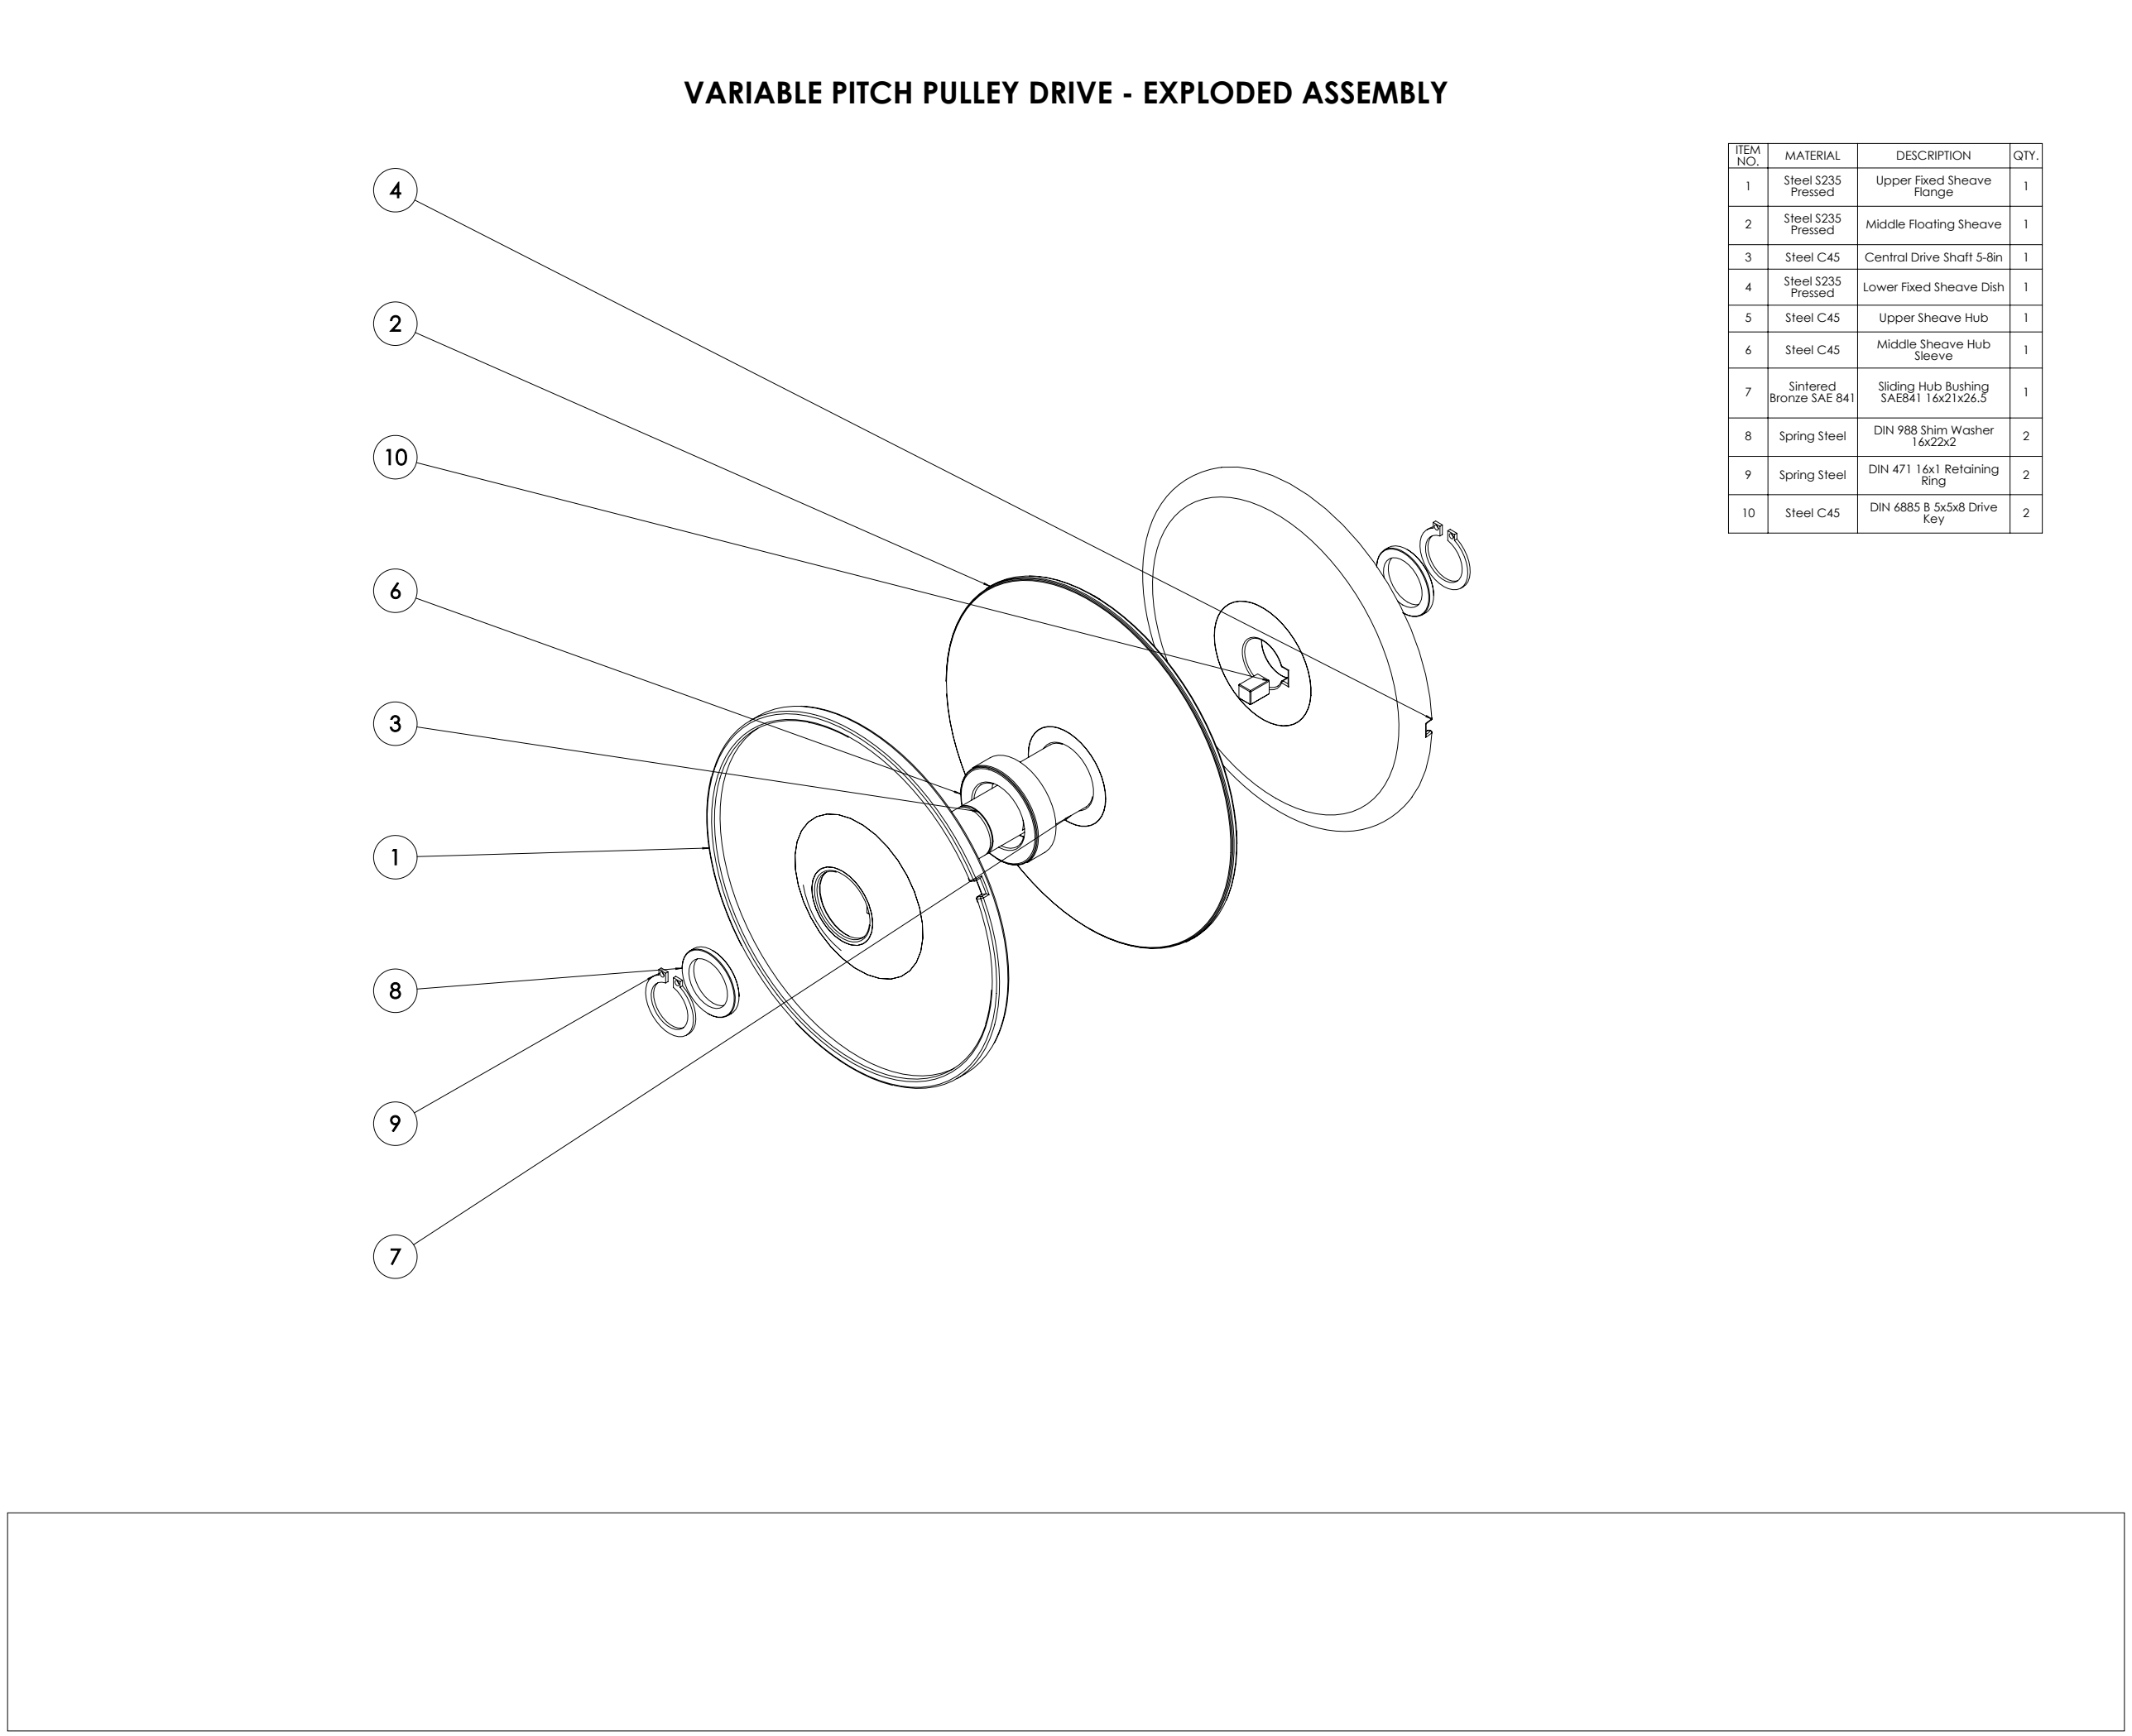
ISO-10303-21;
HEADER;
/* Generated by software containing ST-Developer
 * from STEP Tools, Inc. (www.steptools.com) 
 */

FILE_DESCRIPTION(
/* description */ (''),
/* implementation_level */ '2;1');

FILE_NAME(
/* name */ 'MAS-362',
/* time_stamp */ '2026-10-24T13:41:11-07:00',
/* author */ (''),
/* organization */ (''),
/* preprocessor_version */ 'ST-DEVELOPER v20.2',
/* originating_system */ 'Autodesk Translation Framework v15.15.0.0',
/* authorisation */ '');

FILE_SCHEMA (('AUTOMOTIVE_DESIGN { 1 0 10303 214 3 1 1 }'));
ENDSEC;

DATA;
#10=MECHANICAL_DESIGN_GEOMETRIC_PRESENTATION_REPRESENTATION('',(#121,#122,
#123,#124,#125,#126,#127,#128,#129,#130),#12813);
#11=ITEM_DEFINED_TRANSFORMATION($,$,#4506,#4991);
#12=ITEM_DEFINED_TRANSFORMATION($,$,#4561,#4992);
#13=ITEM_DEFINED_TRANSFORMATION($,$,#4614,#4993);
#14=ITEM_DEFINED_TRANSFORMATION($,$,#4704,#4994);
#15=ITEM_DEFINED_TRANSFORMATION($,$,#4796,#4995);
#16=ITEM_DEFINED_TRANSFORMATION($,$,#4885,#4996);
#17=ITEM_DEFINED_TRANSFORMATION($,$,#4917,#4997);
#18=ITEM_DEFINED_TRANSFORMATION($,$,#4930,#4998);
#19=ITEM_DEFINED_TRANSFORMATION($,$,#4930,#4999);
#20=ITEM_DEFINED_TRANSFORMATION($,$,#4943,#5000);
#21=ITEM_DEFINED_TRANSFORMATION($,$,#4943,#5001);
#22=ITEM_DEFINED_TRANSFORMATION($,$,#4964,#5002);
#23=ITEM_DEFINED_TRANSFORMATION($,$,#4964,#5003);
#24=(
REPRESENTATION_RELATIONSHIP($,$,#12854,#12853)
REPRESENTATION_RELATIONSHIP_WITH_TRANSFORMATION(#11)
SHAPE_REPRESENTATION_RELATIONSHIP()
);
#25=(
REPRESENTATION_RELATIONSHIP($,$,#12855,#12853)
REPRESENTATION_RELATIONSHIP_WITH_TRANSFORMATION(#12)
SHAPE_REPRESENTATION_RELATIONSHIP()
);
#26=(
REPRESENTATION_RELATIONSHIP($,$,#12856,#12853)
REPRESENTATION_RELATIONSHIP_WITH_TRANSFORMATION(#13)
SHAPE_REPRESENTATION_RELATIONSHIP()
);
#27=(
REPRESENTATION_RELATIONSHIP($,$,#12857,#12853)
REPRESENTATION_RELATIONSHIP_WITH_TRANSFORMATION(#14)
SHAPE_REPRESENTATION_RELATIONSHIP()
);
#28=(
REPRESENTATION_RELATIONSHIP($,$,#12858,#12853)
REPRESENTATION_RELATIONSHIP_WITH_TRANSFORMATION(#15)
SHAPE_REPRESENTATION_RELATIONSHIP()
);
#29=(
REPRESENTATION_RELATIONSHIP($,$,#12859,#12853)
REPRESENTATION_RELATIONSHIP_WITH_TRANSFORMATION(#16)
SHAPE_REPRESENTATION_RELATIONSHIP()
);
#30=(
REPRESENTATION_RELATIONSHIP($,$,#12860,#12853)
REPRESENTATION_RELATIONSHIP_WITH_TRANSFORMATION(#17)
SHAPE_REPRESENTATION_RELATIONSHIP()
);
#31=(
REPRESENTATION_RELATIONSHIP($,$,#12861,#12853)
REPRESENTATION_RELATIONSHIP_WITH_TRANSFORMATION(#18)
SHAPE_REPRESENTATION_RELATIONSHIP()
);
#32=(
REPRESENTATION_RELATIONSHIP($,$,#12861,#12853)
REPRESENTATION_RELATIONSHIP_WITH_TRANSFORMATION(#19)
SHAPE_REPRESENTATION_RELATIONSHIP()
);
#33=(
REPRESENTATION_RELATIONSHIP($,$,#12862,#12853)
REPRESENTATION_RELATIONSHIP_WITH_TRANSFORMATION(#20)
SHAPE_REPRESENTATION_RELATIONSHIP()
);
#34=(
REPRESENTATION_RELATIONSHIP($,$,#12862,#12853)
REPRESENTATION_RELATIONSHIP_WITH_TRANSFORMATION(#21)
SHAPE_REPRESENTATION_RELATIONSHIP()
);
#35=(
REPRESENTATION_RELATIONSHIP($,$,#12863,#12853)
REPRESENTATION_RELATIONSHIP_WITH_TRANSFORMATION(#22)
SHAPE_REPRESENTATION_RELATIONSHIP()
);
#36=(
REPRESENTATION_RELATIONSHIP($,$,#12863,#12853)
REPRESENTATION_RELATIONSHIP_WITH_TRANSFORMATION(#23)
SHAPE_REPRESENTATION_RELATIONSHIP()
);
#37=CONTEXT_DEPENDENT_SHAPE_REPRESENTATION(#24,#12840);
#38=CONTEXT_DEPENDENT_SHAPE_REPRESENTATION(#25,#12841);
#39=CONTEXT_DEPENDENT_SHAPE_REPRESENTATION(#26,#12842);
#40=CONTEXT_DEPENDENT_SHAPE_REPRESENTATION(#27,#12843);
#41=CONTEXT_DEPENDENT_SHAPE_REPRESENTATION(#28,#12844);
#42=CONTEXT_DEPENDENT_SHAPE_REPRESENTATION(#29,#12845);
#43=CONTEXT_DEPENDENT_SHAPE_REPRESENTATION(#30,#12846);
#44=CONTEXT_DEPENDENT_SHAPE_REPRESENTATION(#31,#12847);
#45=CONTEXT_DEPENDENT_SHAPE_REPRESENTATION(#32,#12848);
#46=CONTEXT_DEPENDENT_SHAPE_REPRESENTATION(#33,#12849);
#47=CONTEXT_DEPENDENT_SHAPE_REPRESENTATION(#34,#12850);
#48=CONTEXT_DEPENDENT_SHAPE_REPRESENTATION(#35,#12851);
#49=CONTEXT_DEPENDENT_SHAPE_REPRESENTATION(#36,#12852);
#50=NEXT_ASSEMBLY_USAGE_OCCURRENCE('01_Upper_Fixed_Sheave_Flange:2',
'01_Upper_Fixed_Sheave_Flange:2','01_Upper_Fixed_Sheave_Flange:2',#12865,
#12866,'01_Upper_Fixed_Sheave_Flange:2');
#51=NEXT_ASSEMBLY_USAGE_OCCURRENCE('02_Middle_Floating_Sheave:2',
'02_Middle_Floating_Sheave:2','02_Middle_Floating_Sheave:2',#12865,#12867,
'02_Middle_Floating_Sheave:2');
#52=NEXT_ASSEMBLY_USAGE_OCCURRENCE('03_Central_Drive_Shaft_5-8in:2',
'03_Central_Drive_Shaft_5-8in:2','03_Central_Drive_Shaft_5-8in:2',#12865,
#12868,'03_Central_Drive_Shaft_5-8in:2');
#53=NEXT_ASSEMBLY_USAGE_OCCURRENCE('04_Lower_Fixed_Sheave_Dish:2',
'04_Lower_Fixed_Sheave_Dish:2','04_Lower_Fixed_Sheave_Dish:2',#12865,#12869,
'04_Lower_Fixed_Sheave_Dish:2');
#54=NEXT_ASSEMBLY_USAGE_OCCURRENCE('05_Upper_Sheave_Hub:2',
'05_Upper_Sheave_Hub:2','05_Upper_Sheave_Hub:2',#12865,#12870,
'05_Upper_Sheave_Hub:2');
#55=NEXT_ASSEMBLY_USAGE_OCCURRENCE('06_Middle_Sheave_Hub_Sleeve:2',
'06_Middle_Sheave_Hub_Sleeve:2','06_Middle_Sheave_Hub_Sleeve:2',#12865,
#12871,'06_Middle_Sheave_Hub_Sleeve:2');
#56=NEXT_ASSEMBLY_USAGE_OCCURRENCE(
'07_Sliding_Hub_Bushing_SAE841_16x21x26.5:2',
'07_Sliding_Hub_Bushing_SAE841_16x21x26.5:2',
'07_Sliding_Hub_Bushing_SAE841_16x21x26.5:2',#12865,#12872,
'07_Sliding_Hub_Bushing_SAE841_16x21x26.5:2');
#57=NEXT_ASSEMBLY_USAGE_OCCURRENCE('08_DIN_988_Shim_Washer_16x22x2:2',
'08_DIN_988_Shim_Washer_16x22x2:2','08_DIN_988_Shim_Washer_16x22x2:2',#12865,
#12873,'08_DIN_988_Shim_Washer_16x22x2:2');
#58=NEXT_ASSEMBLY_USAGE_OCCURRENCE('08_DIN_988_Shim_Washer_16x22x2:3',
'08_DIN_988_Shim_Washer_16x22x2:3','08_DIN_988_Shim_Washer_16x22x2:3',#12865,
#12873,'08_DIN_988_Shim_Washer_16x22x2:3');
#59=NEXT_ASSEMBLY_USAGE_OCCURRENCE('09_DIN_471_16x1_Retaining_Ring:2',
'09_DIN_471_16x1_Retaining_Ring:2','09_DIN_471_16x1_Retaining_Ring:2',#12865,
#12874,'09_DIN_471_16x1_Retaining_Ring:2');
#60=NEXT_ASSEMBLY_USAGE_OCCURRENCE('09_DIN_471_16x1_Retaining_Ring:3',
'09_DIN_471_16x1_Retaining_Ring:3','09_DIN_471_16x1_Retaining_Ring:3',#12865,
#12874,'09_DIN_471_16x1_Retaining_Ring:3');
#61=NEXT_ASSEMBLY_USAGE_OCCURRENCE('10_DIN_6885_B_5x5x8_Drive_Key:2',
'10_DIN_6885_B_5x5x8_Drive_Key:2','10_DIN_6885_B_5x5x8_Drive_Key:2',#12865,
#12875,'10_DIN_6885_B_5x5x8_Drive_Key:2');
#62=NEXT_ASSEMBLY_USAGE_OCCURRENCE('10_DIN_6885_B_5x5x8_Drive_Key:3',
'10_DIN_6885_B_5x5x8_Drive_Key:3','10_DIN_6885_B_5x5x8_Drive_Key:3',#12865,
#12875,'10_DIN_6885_B_5x5x8_Drive_Key:3');
#63=ELLIPSE('',#4739,0.707106781186547,0.5);
#64=ELLIPSE('',#4740,0.707106781186547,0.5);
#65=ELLIPSE('',#4754,0.707106781186549,0.5);
#66=ELLIPSE('',#4755,0.707106781186547,0.5);
#67=SPHERICAL_SURFACE('',#4710,0.5);
#68=SPHERICAL_SURFACE('',#4712,0.5);
#69=SPHERICAL_SURFACE('',#4720,0.5);
#70=SPHERICAL_SURFACE('',#4723,0.5);
#71=SPHERICAL_SURFACE('',#4743,0.5);
#72=SPHERICAL_SURFACE('',#4756,0.5);
#73=SPHERICAL_SURFACE('',#4773,0.5);
#74=SPHERICAL_SURFACE('',#4779,0.5);
#75=SPHERICAL_SURFACE('',#4788,0.5);
#76=SPHERICAL_SURFACE('',#4790,0.5);
#77=SPHERICAL_SURFACE('',#4848,0.4);
#78=SPHERICAL_SURFACE('',#4850,0.4);
#79=SPHERICAL_SURFACE('',#4873,0.4);
#80=SPHERICAL_SURFACE('',#4876,0.4);
#81=CONICAL_SURFACE('',#4567,37.5,1.36447243276518);
#82=CONICAL_SURFACE('',#4576,59.25,0.785398163397448);
#83=CONICAL_SURFACE('',#4590,59.25,0.785398163397448);
#84=CONICAL_SURFACE('',#4597,37.5,1.39585880542621);
#85=CONICAL_SURFACE('',#4661,1.775,1.02974425867666);
#86=CONICAL_SURFACE('',#4663,3.85,0.785398163397459);
#87=CONICAL_SURFACE('',#4698,7.69,0.785398163397449);
#88=CONICAL_SURFACE('',#4701,7.54,0.785398163397436);
#89=CONICAL_SURFACE('',#4727,35.,1.37340076694502);
#90=CONICAL_SURFACE('',#4770,35.5,1.39833325526807);
#91=CONICAL_SURFACE('',#4795,56.05,0.694738276196701);
#92=CONICAL_SURFACE('',#4797,12.45,0.785398163397445);
#93=CONICAL_SURFACE('',#4806,12.45,0.785398163397445);
#94=CONICAL_SURFACE('',#4828,10.75,0.785398163397451);
#95=CONICAL_SURFACE('',#4840,10.75,0.785398163397451);
#96=CONICAL_SURFACE('',#4891,15.75,0.785398163397451);
#97=CONICAL_SURFACE('',#4923,8.115,0.785398163397445);
#98=CONICAL_SURFACE('',#4927,8.115,0.785398163397448);
#99=CONICAL_SURFACE('',#4931,10.9,0.785398163397449);
#100=CONICAL_SURFACE('',#4936,10.9,0.785398163397448);
#101=SHAPE_REPRESENTATION_RELATIONSHIP('SRR','None',#12854,#111);
#102=SHAPE_REPRESENTATION_RELATIONSHIP('SRR','None',#12855,#112);
#103=SHAPE_REPRESENTATION_RELATIONSHIP('SRR','None',#12856,#113);
#104=SHAPE_REPRESENTATION_RELATIONSHIP('SRR','None',#12857,#114);
#105=SHAPE_REPRESENTATION_RELATIONSHIP('SRR','None',#12858,#115);
#106=SHAPE_REPRESENTATION_RELATIONSHIP('SRR','None',#12859,#116);
#107=SHAPE_REPRESENTATION_RELATIONSHIP('SRR','None',#12860,#117);
#108=SHAPE_REPRESENTATION_RELATIONSHIP('SRR','None',#12861,#118);
#109=SHAPE_REPRESENTATION_RELATIONSHIP('SRR','None',#12862,#119);
#110=SHAPE_REPRESENTATION_RELATIONSHIP('SRR','None',#12863,#120);
#111=ADVANCED_BREP_SHAPE_REPRESENTATION('',(#131),#12803);
#112=ADVANCED_BREP_SHAPE_REPRESENTATION('',(#132),#12804);
#113=ADVANCED_BREP_SHAPE_REPRESENTATION('',(#133),#12805);
#114=ADVANCED_BREP_SHAPE_REPRESENTATION('',(#134),#12806);
#115=ADVANCED_BREP_SHAPE_REPRESENTATION('',(#135),#12807);
#116=ADVANCED_BREP_SHAPE_REPRESENTATION('',(#136),#12808);
#117=ADVANCED_BREP_SHAPE_REPRESENTATION('',(#137),#12809);
#118=ADVANCED_BREP_SHAPE_REPRESENTATION('',(#138),#12810);
#119=ADVANCED_BREP_SHAPE_REPRESENTATION('',(#139),#12811);
#120=ADVANCED_BREP_SHAPE_REPRESENTATION('',(#140),#12812);
#121=STYLED_ITEM('',(#12960),#131);
#122=STYLED_ITEM('',(#12988),#132);
#123=STYLED_ITEM('',(#12974),#133);
#124=STYLED_ITEM('',(#12967),#134);
#125=STYLED_ITEM('',(#12960),#135);
#126=STYLED_ITEM('',(#12960),#136);
#127=STYLED_ITEM('',(#12967),#137);
#128=STYLED_ITEM('',(#12981),#138);
#129=STYLED_ITEM('',(#12988),#139);
#130=STYLED_ITEM('',(#12974),#140);
#131=MANIFOLD_SOLID_BREP('Body1',#4384);
#132=MANIFOLD_SOLID_BREP('Body1',#4385);
#133=MANIFOLD_SOLID_BREP('Body1',#4386);
#134=MANIFOLD_SOLID_BREP('Body1',#4387);
#135=MANIFOLD_SOLID_BREP('Body1',#4388);
#136=MANIFOLD_SOLID_BREP('Body1',#4389);
#137=MANIFOLD_SOLID_BREP('Body1',#4390);
#138=MANIFOLD_SOLID_BREP('Body1',#4391);
#139=MANIFOLD_SOLID_BREP('Body1',#4392);
#140=MANIFOLD_SOLID_BREP('Body1',#4393);
#141=FACE_BOUND('',#599,.T.);
#142=FACE_BOUND('',#604,.T.);
#143=FACE_BOUND('',#607,.T.);
#144=FACE_BOUND('',#632,.T.);
#145=FACE_BOUND('',#643,.T.);
#146=FACE_BOUND('',#701,.T.);
#147=FACE_BOUND('',#704,.T.);
#148=FACE_BOUND('',#706,.T.);
#149=FACE_BOUND('',#707,.T.);
#150=FACE_BOUND('',#709,.T.);
#151=FACE_BOUND('',#712,.T.);
#152=FACE_BOUND('',#719,.T.);
#153=FACE_BOUND('',#738,.T.);
#154=FACE_BOUND('',#753,.T.);
#155=FACE_BOUND('',#774,.T.);
#156=FACE_BOUND('',#779,.T.);
#157=FACE_BOUND('',#782,.T.);
#158=FACE_BOUND('',#811,.T.);
#159=FACE_BOUND('',#825,.T.);
#160=FACE_BOUND('',#830,.T.);
#161=FACE_BOUND('',#836,.T.);
#162=FACE_BOUND('',#841,.T.);
#163=FACE_BOUND('',#846,.T.);
#164=FACE_BOUND('',#849,.T.);
#165=FACE_BOUND('',#853,.T.);
#166=FACE_BOUND('',#854,.T.);
#167=FACE_BOUND('',#859,.T.);
#168=FACE_BOUND('',#860,.T.);
#169=PLANE('',#4514);
#170=PLANE('',#4517);
#171=PLANE('',#4521);
#172=PLANE('',#4531);
#173=PLANE('',#4540);
#174=PLANE('',#4544);
#175=PLANE('',#4551);
#176=PLANE('',#4570);
#177=PLANE('',#4603);
#178=PLANE('',#4654);
#179=PLANE('',#4658);
#180=PLANE('',#4665);
#181=PLANE('',#4666);
#182=PLANE('',#4668);
#183=PLANE('',#4669);
#184=PLANE('',#4671);
#185=PLANE('',#4672);
#186=PLANE('',#4673);
#187=PLANE('',#4675);
#188=PLANE('',#4676);
#189=PLANE('',#4678);
#190=PLANE('',#4679);
#191=PLANE('',#4684);
#192=PLANE('',#4688);
#193=PLANE('',#4692);
#194=PLANE('',#4696);
#195=PLANE('',#4703);
#196=PLANE('',#4717);
#197=PLANE('',#4725);
#198=PLANE('',#4734);
#199=PLANE('',#4751);
#200=PLANE('',#4752);
#201=PLANE('',#4769);
#202=PLANE('',#4781);
#203=PLANE('',#4792);
#204=PLANE('',#4793);
#205=PLANE('',#4794);
#206=PLANE('',#4804);
#207=PLANE('',#4808);
#208=PLANE('',#4816);
#209=PLANE('',#4817);
#210=PLANE('',#4818);
#211=PLANE('',#4819);
#212=PLANE('',#4820);
#213=PLANE('',#4852);
#214=PLANE('',#4855);
#215=PLANE('',#4862);
#216=PLANE('',#4872);
#217=PLANE('',#4884);
#218=PLANE('',#4894);
#219=PLANE('',#4906);
#220=PLANE('',#4921);
#221=PLANE('',#4929);
#222=PLANE('',#4938);
#223=PLANE('',#4942);
#224=PLANE('',#4950);
#225=PLANE('',#4953);
#226=PLANE('',#4954);
#227=PLANE('',#4955);
#228=PLANE('',#4956);
#229=PLANE('',#4960);
#230=PLANE('',#4961);
#231=PLANE('',#4962);
#232=PLANE('',#4965);
#233=PLANE('',#4966);
#234=PLANE('',#4967);
#235=PLANE('',#4968);
#236=PLANE('',#4969);
#237=PLANE('',#4970);
#238=PLANE('',#4971);
#239=PLANE('',#4972);
#240=PLANE('',#4973);
#241=PLANE('',#4974);
#242=PLANE('',#4975);
#243=PLANE('',#4976);
#244=PLANE('',#4977);
#245=PLANE('',#4978);
#246=PLANE('',#4979);
#247=PLANE('',#4980);
#248=PLANE('',#4981);
#249=PLANE('',#4982);
#250=PLANE('',#4983);
#251=PLANE('',#4984);
#252=PLANE('',#4985);
#253=PLANE('',#4986);
#254=PLANE('',#4987);
#255=PLANE('',#4988);
#256=PLANE('',#4989);
#257=PLANE('',#4990);
#258=TOROIDAL_SURFACE('',#4511,11.5,0.5);
#259=TOROIDAL_SURFACE('',#4541,60.,0.5);
#260=TOROIDAL_SURFACE('',#4546,58.,0.5);
#261=TOROIDAL_SURFACE('',#4549,58.1,0.6);
#262=TOROIDAL_SURFACE('',#4558,59.9,0.6);
#263=TOROIDAL_SURFACE('',#4559,59.7,0.8);
#264=TOROIDAL_SURFACE('',#4562,15.9482352626124,0.5);
#265=TOROIDAL_SURFACE('',#4572,58.7517732660432,0.5);
#266=TOROIDAL_SURFACE('',#4579,59.,0.5);
#267=TOROIDAL_SURFACE('',#4586,59.,0.5);
#268=TOROIDAL_SURFACE('',#4593,58.7578429367487,0.5);
#269=TOROIDAL_SURFACE('',#4600,15.9561537431677,0.5);
#270=TOROIDAL_SURFACE('',#4605,11.,0.5);
#271=TOROIDAL_SURFACE('',#4612,11.,0.5);
#272=TOROIDAL_SURFACE('',#4705,56.5341874729922,0.5);
#273=TOROIDAL_SURFACE('',#4729,11.5,0.5);
#274=TOROIDAL_SURFACE('',#4746,8.45,0.5);
#275=TOROIDAL_SURFACE('',#4760,8.45,0.5);
#276=TOROIDAL_SURFACE('',#4764,19.9567770454363,0.5);
#277=TOROIDAL_SURFACE('',#4821,10.6,0.4);
#278=TOROIDAL_SURFACE('',#4831,10.6,0.4);
#279=TOROIDAL_SURFACE('',#4838,10.6,0.4);
#280=TOROIDAL_SURFACE('',#4844,10.3343145750508,0.4);
#281=TOROIDAL_SURFACE('',#4859,10.3343145750508,0.4);
#282=TOROIDAL_SURFACE('',#4864,8.35,0.4);
#283=TOROIDAL_SURFACE('',#4879,8.35,0.4);
#284=TOROIDAL_SURFACE('',#4881,8.35,0.4);
#285=TOROIDAL_SURFACE('',#4886,15.2928932188134,0.5);
#286=TOROIDAL_SURFACE('',#4896,15.5,0.5);
#287=TOROIDAL_SURFACE('',#4903,15.5,0.5);
#288=TOROIDAL_SURFACE('',#4908,11.,0.5);
#289=TOROIDAL_SURFACE('',#4915,11.,0.5);
#290=(
BOUNDED_CURVE()
B_SPLINE_CURVE(5,(#6647,#6648,#6649,#6650,#6651,#6652,#6653,#6654,#6655,
#6656,#6657,#6658,#6659,#6660,#6661,#6662,#6663,#6664,#6665,#6666,#6667,
#6668,#6669,#6670,#6671,#6672,#6673,#6674,#6675,#6676),.UNSPECIFIED.,.F.,
 .F.)
B_SPLINE_CURVE_WITH_KNOTS((6,1,1,1,1,1,1,1,1,1,1,1,1,1,1,1,1,1,1,1,1,1,
1,1,1,6),(8.37815962158244E-5,0.04,0.08,0.12,0.16,0.2,0.24,0.28,0.32,0.36,
0.4,0.44,0.48,0.52,0.56,0.6,0.64,0.68,0.72,0.76,0.8,0.84,0.88,0.92,0.96,
0.969915757295795),.UNSPECIFIED.)
CURVE()
GEOMETRIC_REPRESENTATION_ITEM()
RATIONAL_B_SPLINE_CURVE((1.,1.,1.,1.,1.,1.,1.,1.,1.,1.,1.,1.,1.,1.,1.,1.,
1.,1.,1.,1.,1.,1.,1.,1.,1.,1.,1.,1.,1.,1.))
REPRESENTATION_ITEM('')
);
#291=(
BOUNDED_CURVE()
B_SPLINE_CURVE(5,(#7077,#7078,#7079,#7080,#7081,#7082,#7083,#7084,#7085,
#7086,#7087,#7088,#7089,#7090,#7091,#7092,#7093,#7094,#7095,#7096,#7097,
#7098,#7099,#7100,#7101,#7102,#7103,#7104,#7105,#7106),.UNSPECIFIED.,.F.,
 .F.)
B_SPLINE_CURVE_WITH_KNOTS((6,1,1,1,1,1,1,1,1,1,1,1,1,1,1,1,1,1,1,1,1,1,
1,1,1,6),(0.00142562377953934,0.04,0.08,0.12,0.16,0.2,0.24,0.28,0.32,0.36,
0.4,0.44,0.48,0.52,0.56,0.6,0.64,0.68,0.72,0.76,0.8,0.84,0.88,0.92,0.96,
0.999682925140619),.UNSPECIFIED.)
CURVE()
GEOMETRIC_REPRESENTATION_ITEM()
RATIONAL_B_SPLINE_CURVE((1.,1.,1.,1.,1.,1.,1.,1.,1.,1.,1.,1.,1.,1.,1.,1.,
1.,1.,1.,1.,1.,1.,1.,1.,1.,1.,1.,1.,1.,1.))
REPRESENTATION_ITEM('')
);
#292=(
BOUNDED_CURVE()
B_SPLINE_CURVE(5,(#10926,#10927,#10928,#10929,#10930,#10931,#10932,#10933,
#10934,#10935,#10936,#10937,#10938,#10939,#10940),.UNSPECIFIED.,.F.,.F.)
B_SPLINE_CURVE_WITH_KNOTS((6,1,1,1,1,1,1,1,1,1,6),(0.000900413620571326,
0.0666666666666667,0.133333333333333,0.2,0.266666666666667,0.333333333333333,
0.4,0.466666666666667,0.533333333333333,0.6,0.62572757688512),
 .UNSPECIFIED.)
CURVE()
GEOMETRIC_REPRESENTATION_ITEM()
RATIONAL_B_SPLINE_CURVE((1.,1.,1.,1.,1.,1.,1.,1.,1.,1.,1.,1.,1.,1.,1.))
REPRESENTATION_ITEM('')
);
#293=(
BOUNDED_CURVE()
B_SPLINE_CURVE(5,(#11656,#11657,#11658,#11659,#11660,#11661,#11662,#11663,
#11664,#11665,#11666,#11667,#11668,#11669,#11670,#11671,#11672,#11673,#11674),
 .UNSPECIFIED.,.F.,.F.)
B_SPLINE_CURVE_WITH_KNOTS((6,1,1,1,1,1,1,1,1,1,1,1,1,1,6),(0.323025444096601,
0.35,0.4,0.45,0.5,0.55,0.6,0.65,0.7,0.75,0.8,0.85,0.9,0.95,1.),
 .UNSPECIFIED.)
CURVE()
GEOMETRIC_REPRESENTATION_ITEM()
RATIONAL_B_SPLINE_CURVE((1.,1.,1.,1.,1.,1.,1.,1.,1.,1.,1.,1.,1.,1.,1.,1.,
1.,1.,1.))
REPRESENTATION_ITEM('')
);
#294=(
BOUNDED_SURFACE()
B_SPLINE_SURFACE(5,2,((#6376,#6377,#6378,#6379,#6380,#6381,#6382,#6383,
#6384),(#6385,#6386,#6387,#6388,#6389,#6390,#6391,#6392,#6393),(#6394,#6395,
#6396,#6397,#6398,#6399,#6400,#6401,#6402),(#6403,#6404,#6405,#6406,#6407,
#6408,#6409,#6410,#6411),(#6412,#6413,#6414,#6415,#6416,#6417,#6418,#6419,
#6420),(#6421,#6422,#6423,#6424,#6425,#6426,#6427,#6428,#6429),(#6430,#6431,
#6432,#6433,#6434,#6435,#6436,#6437,#6438),(#6439,#6440,#6441,#6442,#6443,
#6444,#6445,#6446,#6447),(#6448,#6449,#6450,#6451,#6452,#6453,#6454,#6455,
#6456),(#6457,#6458,#6459,#6460,#6461,#6462,#6463,#6464,#6465),(#6466,#6467,
#6468,#6469,#6470,#6471,#6472,#6473,#6474),(#6475,#6476,#6477,#6478,#6479,
#6480,#6481,#6482,#6483),(#6484,#6485,#6486,#6487,#6488,#6489,#6490,#6491,
#6492),(#6493,#6494,#6495,#6496,#6497,#6498,#6499,#6500,#6501),(#6502,#6503,
#6504,#6505,#6506,#6507,#6508,#6509,#6510),(#6511,#6512,#6513,#6514,#6515,
#6516,#6517,#6518,#6519),(#6520,#6521,#6522,#6523,#6524,#6525,#6526,#6527,
#6528),(#6529,#6530,#6531,#6532,#6533,#6534,#6535,#6536,#6537),(#6538,#6539,
#6540,#6541,#6542,#6543,#6544,#6545,#6546),(#6547,#6548,#6549,#6550,#6551,
#6552,#6553,#6554,#6555),(#6556,#6557,#6558,#6559,#6560,#6561,#6562,#6563,
#6564),(#6565,#6566,#6567,#6568,#6569,#6570,#6571,#6572,#6573),(#6574,#6575,
#6576,#6577,#6578,#6579,#6580,#6581,#6582),(#6583,#6584,#6585,#6586,#6587,
#6588,#6589,#6590,#6591),(#6592,#6593,#6594,#6595,#6596,#6597,#6598,#6599,
#6600),(#6601,#6602,#6603,#6604,#6605,#6606,#6607,#6608,#6609),(#6610,#6611,
#6612,#6613,#6614,#6615,#6616,#6617,#6618),(#6619,#6620,#6621,#6622,#6623,
#6624,#6625,#6626,#6627),(#6628,#6629,#6630,#6631,#6632,#6633,#6634,#6635,
#6636),(#6637,#6638,#6639,#6640,#6641,#6642,#6643,#6644,#6645)),
 .UNSPECIFIED.,.F.,.T.,.F.)
B_SPLINE_SURFACE_WITH_KNOTS((6,1,1,1,1,1,1,1,1,1,1,1,1,1,1,1,1,1,1,1,1,
1,1,1,1,6),(3,2,2,2,3),(0.,0.04,0.08,0.12,0.16,0.2,0.24,0.28,0.32,0.36,
0.4,0.44,0.48,0.52,0.56,0.6,0.64,0.68,0.72,0.76,0.8,0.84,0.88,0.92,0.96,
1.),(0.,1.5707963267949,3.14159265358979,4.71238898038469,6.28318530717959),
 .UNSPECIFIED.)
GEOMETRIC_REPRESENTATION_ITEM()
RATIONAL_B_SPLINE_SURFACE(((1.,0.707106781186548,1.,0.707106781186548,1.,
0.707106781186548,1.,0.707106781186548,1.),(1.,0.707106781186548,1.,0.707106781186548,
1.,0.707106781186548,1.,0.707106781186548,1.),(1.,0.707106781186548,1.,
0.707106781186548,1.,0.707106781186548,1.,0.707106781186548,1.),(1.,0.707106781186548,
1.,0.707106781186548,1.,0.707106781186548,1.,0.707106781186548,1.),(1.,
0.707106781186548,1.,0.707106781186548,1.,0.707106781186548,1.,0.707106781186548,
1.),(1.,0.707106781186548,1.,0.707106781186548,1.,0.707106781186548,1.,
0.707106781186548,1.),(1.,0.707106781186548,1.,0.707106781186548,1.,0.707106781186548,
1.,0.707106781186548,1.),(1.,0.707106781186548,1.,0.707106781186548,1.,
0.707106781186548,1.,0.707106781186548,1.),(1.,0.707106781186548,1.,0.707106781186548,
1.,0.707106781186548,1.,0.707106781186548,1.),(1.,0.707106781186548,1.,
0.707106781186548,1.,0.707106781186548,1.,0.707106781186548,1.),(1.,0.707106781186548,
1.,0.707106781186548,1.,0.707106781186548,1.,0.707106781186548,1.),(1.,
0.707106781186548,1.,0.707106781186548,1.,0.707106781186548,1.,0.707106781186548,
1.),(1.,0.707106781186548,1.,0.707106781186548,1.,0.707106781186548,1.,
0.707106781186548,1.),(1.,0.707106781186548,1.,0.707106781186548,1.,0.707106781186548,
1.,0.707106781186548,1.),(1.,0.707106781186548,1.,0.707106781186548,1.,
0.707106781186548,1.,0.707106781186548,1.),(1.,0.707106781186548,1.,0.707106781186548,
1.,0.707106781186548,1.,0.707106781186548,1.),(1.,0.707106781186548,1.,
0.707106781186548,1.,0.707106781186548,1.,0.707106781186548,1.),(1.,0.707106781186548,
1.,0.707106781186548,1.,0.707106781186548,1.,0.707106781186548,1.),(1.,
0.707106781186548,1.,0.707106781186548,1.,0.707106781186548,1.,0.707106781186548,
1.),(1.,0.707106781186548,1.,0.707106781186548,1.,0.707106781186548,1.,
0.707106781186548,1.),(1.,0.707106781186548,1.,0.707106781186548,1.,0.707106781186548,
1.,0.707106781186548,1.),(1.,0.707106781186548,1.,0.707106781186548,1.,
0.707106781186548,1.,0.707106781186548,1.),(1.,0.707106781186548,1.,0.707106781186548,
1.,0.707106781186548,1.,0.707106781186548,1.),(1.,0.707106781186548,1.,
0.707106781186548,1.,0.707106781186548,1.,0.707106781186548,1.),(1.,0.707106781186548,
1.,0.707106781186548,1.,0.707106781186548,1.,0.707106781186548,1.),(1.,
0.707106781186548,1.,0.707106781186548,1.,0.707106781186548,1.,0.707106781186548,
1.),(1.,0.707106781186548,1.,0.707106781186548,1.,0.707106781186548,1.,
0.707106781186548,1.),(1.,0.707106781186548,1.,0.707106781186548,1.,0.707106781186548,
1.,0.707106781186548,1.),(1.,0.707106781186548,1.,0.707106781186548,1.,
0.707106781186548,1.,0.707106781186548,1.),(1.,0.707106781186548,1.,0.707106781186548,
1.,0.707106781186548,1.,0.707106781186548,1.)))
REPRESENTATION_ITEM('')
SURFACE()
);
#295=(
BOUNDED_SURFACE()
B_SPLINE_SURFACE(5,2,((#6806,#6807,#6808,#6809,#6810,#6811,#6812,#6813,
#6814),(#6815,#6816,#6817,#6818,#6819,#6820,#6821,#6822,#6823),(#6824,#6825,
#6826,#6827,#6828,#6829,#6830,#6831,#6832),(#6833,#6834,#6835,#6836,#6837,
#6838,#6839,#6840,#6841),(#6842,#6843,#6844,#6845,#6846,#6847,#6848,#6849,
#6850),(#6851,#6852,#6853,#6854,#6855,#6856,#6857,#6858,#6859),(#6860,#6861,
#6862,#6863,#6864,#6865,#6866,#6867,#6868),(#6869,#6870,#6871,#6872,#6873,
#6874,#6875,#6876,#6877),(#6878,#6879,#6880,#6881,#6882,#6883,#6884,#6885,
#6886),(#6887,#6888,#6889,#6890,#6891,#6892,#6893,#6894,#6895),(#6896,#6897,
#6898,#6899,#6900,#6901,#6902,#6903,#6904),(#6905,#6906,#6907,#6908,#6909,
#6910,#6911,#6912,#6913),(#6914,#6915,#6916,#6917,#6918,#6919,#6920,#6921,
#6922),(#6923,#6924,#6925,#6926,#6927,#6928,#6929,#6930,#6931),(#6932,#6933,
#6934,#6935,#6936,#6937,#6938,#6939,#6940),(#6941,#6942,#6943,#6944,#6945,
#6946,#6947,#6948,#6949),(#6950,#6951,#6952,#6953,#6954,#6955,#6956,#6957,
#6958),(#6959,#6960,#6961,#6962,#6963,#6964,#6965,#6966,#6967),(#6968,#6969,
#6970,#6971,#6972,#6973,#6974,#6975,#6976),(#6977,#6978,#6979,#6980,#6981,
#6982,#6983,#6984,#6985),(#6986,#6987,#6988,#6989,#6990,#6991,#6992,#6993,
#6994),(#6995,#6996,#6997,#6998,#6999,#7000,#7001,#7002,#7003),(#7004,#7005,
#7006,#7007,#7008,#7009,#7010,#7011,#7012),(#7013,#7014,#7015,#7016,#7017,
#7018,#7019,#7020,#7021),(#7022,#7023,#7024,#7025,#7026,#7027,#7028,#7029,
#7030),(#7031,#7032,#7033,#7034,#7035,#7036,#7037,#7038,#7039),(#7040,#7041,
#7042,#7043,#7044,#7045,#7046,#7047,#7048),(#7049,#7050,#7051,#7052,#7053,
#7054,#7055,#7056,#7057),(#7058,#7059,#7060,#7061,#7062,#7063,#7064,#7065,
#7066),(#7067,#7068,#7069,#7070,#7071,#7072,#7073,#7074,#7075)),
 .UNSPECIFIED.,.F.,.T.,.F.)
B_SPLINE_SURFACE_WITH_KNOTS((6,1,1,1,1,1,1,1,1,1,1,1,1,1,1,1,1,1,1,1,1,
1,1,1,1,6),(3,2,2,2,3),(0.,0.04,0.08,0.12,0.16,0.2,0.24,0.28,0.32,0.36,
0.4,0.44,0.48,0.52,0.56,0.6,0.64,0.68,0.72,0.76,0.8,0.84,0.88,0.92,0.96,
1.),(0.,1.5707963267949,3.14159265358979,4.71238898038469,6.28318530717959),
 .UNSPECIFIED.)
GEOMETRIC_REPRESENTATION_ITEM()
RATIONAL_B_SPLINE_SURFACE(((1.,0.707106781186548,1.,0.707106781186548,1.,
0.707106781186548,1.,0.707106781186548,1.),(1.,0.707106781186548,1.,0.707106781186548,
1.,0.707106781186548,1.,0.707106781186548,1.),(1.,0.707106781186548,1.,
0.707106781186548,1.,0.707106781186548,1.,0.707106781186548,1.),(1.,0.707106781186548,
1.,0.707106781186548,1.,0.707106781186548,1.,0.707106781186548,1.),(1.,
0.707106781186548,1.,0.707106781186548,1.,0.707106781186548,1.,0.707106781186548,
1.),(1.,0.707106781186548,1.,0.707106781186548,1.,0.707106781186548,1.,
0.707106781186548,1.),(1.,0.707106781186548,1.,0.707106781186548,1.,0.707106781186548,
1.,0.707106781186548,1.),(1.,0.707106781186548,1.,0.707106781186548,1.,
0.707106781186548,1.,0.707106781186548,1.),(1.,0.707106781186548,1.,0.707106781186548,
1.,0.707106781186548,1.,0.707106781186548,1.),(1.,0.707106781186548,1.,
0.707106781186548,1.,0.707106781186548,1.,0.707106781186548,1.),(1.,0.707106781186548,
1.,0.707106781186548,1.,0.707106781186548,1.,0.707106781186548,1.),(1.,
0.707106781186548,1.,0.707106781186548,1.,0.707106781186548,1.,0.707106781186548,
1.),(1.,0.707106781186548,1.,0.707106781186548,1.,0.707106781186548,1.,
0.707106781186548,1.),(1.,0.707106781186548,1.,0.707106781186548,1.,0.707106781186548,
1.,0.707106781186548,1.),(1.,0.707106781186548,1.,0.707106781186548,1.,
0.707106781186548,1.,0.707106781186548,1.),(1.,0.707106781186548,1.,0.707106781186548,
1.,0.707106781186548,1.,0.707106781186548,1.),(1.,0.707106781186548,1.,
0.707106781186548,1.,0.707106781186548,1.,0.707106781186548,1.),(1.,0.707106781186548,
1.,0.707106781186548,1.,0.707106781186548,1.,0.707106781186548,1.),(1.,
0.707106781186548,1.,0.707106781186548,1.,0.707106781186548,1.,0.707106781186548,
1.),(1.,0.707106781186548,1.,0.707106781186548,1.,0.707106781186548,1.,
0.707106781186548,1.),(1.,0.707106781186548,1.,0.707106781186548,1.,0.707106781186548,
1.,0.707106781186548,1.),(1.,0.707106781186548,1.,0.707106781186548,1.,
0.707106781186548,1.,0.707106781186548,1.),(1.,0.707106781186548,1.,0.707106781186548,
1.,0.707106781186548,1.,0.707106781186548,1.),(1.,0.707106781186548,1.,
0.707106781186548,1.,0.707106781186548,1.,0.707106781186548,1.),(1.,0.707106781186548,
1.,0.707106781186548,1.,0.707106781186548,1.,0.707106781186548,1.),(1.,
0.707106781186548,1.,0.707106781186548,1.,0.707106781186548,1.,0.707106781186548,
1.),(1.,0.707106781186548,1.,0.707106781186548,1.,0.707106781186548,1.,
0.707106781186548,1.),(1.,0.707106781186548,1.,0.707106781186548,1.,0.707106781186548,
1.,0.707106781186548,1.),(1.,0.707106781186548,1.,0.707106781186548,1.,
0.707106781186548,1.,0.707106781186548,1.),(1.,0.707106781186548,1.,0.707106781186548,
1.,0.707106781186548,1.,0.707106781186548,1.)))
REPRESENTATION_ITEM('')
SURFACE()
);
#296=(
BOUNDED_SURFACE()
B_SPLINE_SURFACE(5,2,((#10735,#10736,#10737,#10738,#10739,#10740,#10741,
#10742,#10743),(#10744,#10745,#10746,#10747,#10748,#10749,#10750,#10751,
#10752),(#10753,#10754,#10755,#10756,#10757,#10758,#10759,#10760,#10761),
(#10762,#10763,#10764,#10765,#10766,#10767,#10768,#10769,#10770),(#10771,
#10772,#10773,#10774,#10775,#10776,#10777,#10778,#10779),(#10780,#10781,
#10782,#10783,#10784,#10785,#10786,#10787,#10788),(#10789,#10790,#10791,
#10792,#10793,#10794,#10795,#10796,#10797),(#10798,#10799,#10800,#10801,
#10802,#10803,#10804,#10805,#10806),(#10807,#10808,#10809,#10810,#10811,
#10812,#10813,#10814,#10815),(#10816,#10817,#10818,#10819,#10820,#10821,
#10822,#10823,#10824),(#10825,#10826,#10827,#10828,#10829,#10830,#10831,
#10832,#10833),(#10834,#10835,#10836,#10837,#10838,#10839,#10840,#10841,
#10842),(#10843,#10844,#10845,#10846,#10847,#10848,#10849,#10850,#10851),
(#10852,#10853,#10854,#10855,#10856,#10857,#10858,#10859,#10860),(#10861,
#10862,#10863,#10864,#10865,#10866,#10867,#10868,#10869),(#10870,#10871,
#10872,#10873,#10874,#10875,#10876,#10877,#10878),(#10879,#10880,#10881,
#10882,#10883,#10884,#10885,#10886,#10887),(#10888,#10889,#10890,#10891,
#10892,#10893,#10894,#10895,#10896),(#10897,#10898,#10899,#10900,#10901,
#10902,#10903,#10904,#10905),(#10906,#10907,#10908,#10909,#10910,#10911,
#10912,#10913,#10914)),.UNSPECIFIED.,.F.,.T.,.F.)
B_SPLINE_SURFACE_WITH_KNOTS((6,1,1,1,1,1,1,1,1,1,1,1,1,1,1,6),(3,2,2,2,
3),(-1.,-0.933333333333333,-0.866666666666667,-0.8,-0.733333333333333,-0.666666666666667,
-0.6,-0.533333333333333,-0.466666666666667,-0.4,-0.333333333333333,-0.266666666666667,
-0.2,-0.133333333333333,-0.0666666666666667,0.),(0.,1.5707963267949,3.14159265358979,
4.71238898038469,6.28318530717959),.UNSPECIFIED.)
GEOMETRIC_REPRESENTATION_ITEM()
RATIONAL_B_SPLINE_SURFACE(((1.,0.707106781186548,1.,0.707106781186548,1.,
0.707106781186548,1.,0.707106781186548,1.),(1.,0.707106781186548,1.,0.707106781186548,
1.,0.707106781186548,1.,0.707106781186548,1.),(1.,0.707106781186548,1.,
0.707106781186548,1.,0.707106781186548,1.,0.707106781186548,1.),(1.,0.707106781186548,
1.,0.707106781186548,1.,0.707106781186548,1.,0.707106781186548,1.),(1.,
0.707106781186548,1.,0.707106781186548,1.,0.707106781186548,1.,0.707106781186548,
1.),(1.,0.707106781186548,1.,0.707106781186548,1.,0.707106781186548,1.,
0.707106781186548,1.),(1.,0.707106781186548,1.,0.707106781186548,1.,0.707106781186548,
1.,0.707106781186548,1.),(1.,0.707106781186548,1.,0.707106781186548,1.,
0.707106781186548,1.,0.707106781186548,1.),(1.,0.707106781186548,1.,0.707106781186548,
1.,0.707106781186548,1.,0.707106781186548,1.),(1.,0.707106781186548,1.,
0.707106781186548,1.,0.707106781186548,1.,0.707106781186548,1.),(1.,0.707106781186548,
1.,0.707106781186548,1.,0.707106781186548,1.,0.707106781186548,1.),(1.,
0.707106781186548,1.,0.707106781186548,1.,0.707106781186548,1.,0.707106781186548,
1.),(1.,0.707106781186548,1.,0.707106781186548,1.,0.707106781186548,1.,
0.707106781186548,1.),(1.,0.707106781186548,1.,0.707106781186548,1.,0.707106781186548,
1.,0.707106781186548,1.),(1.,0.707106781186548,1.,0.707106781186548,1.,
0.707106781186548,1.,0.707106781186548,1.),(1.,0.707106781186548,1.,0.707106781186548,
1.,0.707106781186548,1.,0.707106781186548,1.),(1.,0.707106781186548,1.,
0.707106781186548,1.,0.707106781186548,1.,0.707106781186548,1.),(1.,0.707106781186548,
1.,0.707106781186548,1.,0.707106781186548,1.,0.707106781186548,1.),(1.,
0.707106781186548,1.,0.707106781186548,1.,0.707106781186548,1.,0.707106781186548,
1.),(1.,0.707106781186548,1.,0.707106781186548,1.,0.707106781186548,1.,
0.707106781186548,1.)))
REPRESENTATION_ITEM('')
SURFACE()
);
#297=(
BOUNDED_SURFACE()
B_SPLINE_SURFACE(5,2,((#11421,#11422,#11423,#11424,#11425,#11426,#11427,
#11428,#11429),(#11430,#11431,#11432,#11433,#11434,#11435,#11436,#11437,
#11438),(#11439,#11440,#11441,#11442,#11443,#11444,#11445,#11446,#11447),
(#11448,#11449,#11450,#11451,#11452,#11453,#11454,#11455,#11456),(#11457,
#11458,#11459,#11460,#11461,#11462,#11463,#11464,#11465),(#11466,#11467,
#11468,#11469,#11470,#11471,#11472,#11473,#11474),(#11475,#11476,#11477,
#11478,#11479,#11480,#11481,#11482,#11483),(#11484,#11485,#11486,#11487,
#11488,#11489,#11490,#11491,#11492),(#11493,#11494,#11495,#11496,#11497,
#11498,#11499,#11500,#11501),(#11502,#11503,#11504,#11505,#11506,#11507,
#11508,#11509,#11510),(#11511,#11512,#11513,#11514,#11515,#11516,#11517,
#11518,#11519),(#11520,#11521,#11522,#11523,#11524,#11525,#11526,#11527,
#11528),(#11529,#11530,#11531,#11532,#11533,#11534,#11535,#11536,#11537),
(#11538,#11539,#11540,#11541,#11542,#11543,#11544,#11545,#11546),(#11547,
#11548,#11549,#11550,#11551,#11552,#11553,#11554,#11555),(#11556,#11557,
#11558,#11559,#11560,#11561,#11562,#11563,#11564),(#11565,#11566,#11567,
#11568,#11569,#11570,#11571,#11572,#11573),(#11574,#11575,#11576,#11577,
#11578,#11579,#11580,#11581,#11582),(#11583,#11584,#11585,#11586,#11587,
#11588,#11589,#11590,#11591),(#11592,#11593,#11594,#11595,#11596,#11597,
#11598,#11599,#11600),(#11601,#11602,#11603,#11604,#11605,#11606,#11607,
#11608,#11609),(#11610,#11611,#11612,#11613,#11614,#11615,#11616,#11617,
#11618),(#11619,#11620,#11621,#11622,#11623,#11624,#11625,#11626,#11627),
(#11628,#11629,#11630,#11631,#11632,#11633,#11634,#11635,#11636),(#11637,
#11638,#11639,#11640,#11641,#11642,#11643,#11644,#11645)),.UNSPECIFIED.,
 .F.,.T.,.F.)
B_SPLINE_SURFACE_WITH_KNOTS((6,1,1,1,1,1,1,1,1,1,1,1,1,1,1,1,1,1,1,1,6),
(3,2,2,2,3),(-1.,-0.95,-0.9,-0.85,-0.8,-0.75,-0.7,-0.65,-0.6,-0.55,-0.5,
-0.45,-0.4,-0.35,-0.3,-0.25,-0.2,-0.15,-0.1,-0.05,0.),(0.,1.5707963267949,
3.14159265358979,4.71238898038469,6.28318530717959),.UNSPECIFIED.)
GEOMETRIC_REPRESENTATION_ITEM()
RATIONAL_B_SPLINE_SURFACE(((1.,0.707106781186548,1.,0.707106781186548,1.,
0.707106781186548,1.,0.707106781186548,1.),(1.,0.707106781186548,1.,0.707106781186548,
1.,0.707106781186548,1.,0.707106781186548,1.),(1.,0.707106781186548,1.,
0.707106781186548,1.,0.707106781186548,1.,0.707106781186548,1.),(1.,0.707106781186548,
1.,0.707106781186548,1.,0.707106781186548,1.,0.707106781186548,1.),(1.,
0.707106781186548,1.,0.707106781186548,1.,0.707106781186548,1.,0.707106781186548,
1.),(1.,0.707106781186548,1.,0.707106781186548,1.,0.707106781186548,1.,
0.707106781186548,1.),(1.,0.707106781186548,1.,0.707106781186548,1.,0.707106781186548,
1.,0.707106781186548,1.),(1.,0.707106781186548,1.,0.707106781186548,1.,
0.707106781186548,1.,0.707106781186548,1.),(1.,0.707106781186548,1.,0.707106781186548,
1.,0.707106781186548,1.,0.707106781186548,1.),(1.,0.707106781186548,1.,
0.707106781186548,1.,0.707106781186548,1.,0.707106781186548,1.),(1.,0.707106781186548,
1.,0.707106781186548,1.,0.707106781186548,1.,0.707106781186548,1.),(1.,
0.707106781186548,1.,0.707106781186548,1.,0.707106781186548,1.,0.707106781186548,
1.),(1.,0.707106781186548,1.,0.707106781186548,1.,0.707106781186548,1.,
0.707106781186548,1.),(1.,0.707106781186548,1.,0.707106781186548,1.,0.707106781186548,
1.,0.707106781186548,1.),(1.,0.707106781186548,1.,0.707106781186548,1.,
0.707106781186548,1.,0.707106781186548,1.),(1.,0.707106781186548,1.,0.707106781186548,
1.,0.707106781186548,1.,0.707106781186548,1.),(1.,0.707106781186548,1.,
0.707106781186548,1.,0.707106781186548,1.,0.707106781186548,1.),(1.,0.707106781186548,
1.,0.707106781186548,1.,0.707106781186548,1.,0.707106781186548,1.),(1.,
0.707106781186548,1.,0.707106781186548,1.,0.707106781186548,1.,0.707106781186548,
1.),(1.,0.707106781186548,1.,0.707106781186548,1.,0.707106781186548,1.,
0.707106781186548,1.),(1.,0.707106781186548,1.,0.707106781186548,1.,0.707106781186548,
1.,0.707106781186548,1.),(1.,0.707106781186548,1.,0.707106781186548,1.,
0.707106781186548,1.,0.707106781186548,1.),(1.,0.707106781186548,1.,0.707106781186548,
1.,0.707106781186548,1.,0.707106781186548,1.),(1.,0.707106781186548,1.,
0.707106781186548,1.,0.707106781186548,1.,0.707106781186548,1.),(1.,0.707106781186548,
1.,0.707106781186548,1.,0.707106781186548,1.,0.707106781186548,1.)))
REPRESENTATION_ITEM('')
SURFACE()
);
#298=B_SPLINE_SURFACE_WITH_KNOTS('',3,3,((#6289,#6290,#6291,#6292,#6293,
#6294,#6295,#6296,#6297,#6298,#6299,#6300,#6301,#6302,#6303,#6304,#6305),
(#6306,#6307,#6308,#6309,#6310,#6311,#6312,#6313,#6314,#6315,#6316,#6317,
#6318,#6319,#6320,#6321,#6322),(#6323,#6324,#6325,#6326,#6327,#6328,#6329,
#6330,#6331,#6332,#6333,#6334,#6335,#6336,#6337,#6338,#6339),(#6340,#6341,
#6342,#6343,#6344,#6345,#6346,#6347,#6348,#6349,#6350,#6351,#6352,#6353,
#6354,#6355,#6356)),.UNSPECIFIED.,.F.,.T.,.F.,(4,4),(4,1,1,1,1,1,1,1,1,
1,1,1,1,1,4),(0.316273000492814,1.),(1.5707963267949,2.01959527730772,2.46839422782055,
2.91719317833338,3.36599212884621,3.96439072952998,4.26359002987186,4.56278933021375,
5.16118793089752,5.4603872312394,6.05878583192317,6.35798513226506,6.95638373294883,
7.40518268346166,7.85398163397448),.UNSPECIFIED.);
#299=B_SPLINE_SURFACE_WITH_KNOTS('',3,3,((#6719,#6720,#6721,#6722,#6723,
#6724,#6725,#6726,#6727,#6728,#6729,#6730,#6731,#6732,#6733,#6734,#6735),
(#6736,#6737,#6738,#6739,#6740,#6741,#6742,#6743,#6744,#6745,#6746,#6747,
#6748,#6749,#6750,#6751,#6752),(#6753,#6754,#6755,#6756,#6757,#6758,#6759,
#6760,#6761,#6762,#6763,#6764,#6765,#6766,#6767,#6768,#6769),(#6770,#6771,
#6772,#6773,#6774,#6775,#6776,#6777,#6778,#6779,#6780,#6781,#6782,#6783,
#6784,#6785,#6786)),.UNSPECIFIED.,.F.,.T.,.F.,(4,4),(4,1,1,1,1,1,1,1,1,
1,1,1,1,1,4),(0.,1.),(1.5707963267949,2.01959527730772,2.46839422782055,
2.91719317833338,3.36599212884621,3.66519142918809,4.26359002987186,4.56278933021375,
5.16118793089752,5.4603872312394,6.05878583192317,6.35798513226506,6.95638373294883,
7.40518268346166,7.85398163397448),.UNSPECIFIED.);
#300=B_SPLINE_SURFACE_WITH_KNOTS('',3,3,((#7126,#7127,#7128,#7129,#7130,
#7131,#7132,#7133,#7134,#7135,#7136,#7137,#7138,#7139,#7140,#7141,#7142,
#7143,#7144),(#7145,#7146,#7147,#7148,#7149,#7150,#7151,#7152,#7153,#7154,
#7155,#7156,#7157,#7158,#7159,#7160,#7161,#7162,#7163),(#7164,#7165,#7166,
#7167,#7168,#7169,#7170,#7171,#7172,#7173,#7174,#7175,#7176,#7177,#7178,
#7179,#7180,#7181,#7182),(#7183,#7184,#7185,#7186,#7187,#7188,#7189,#7190,
#7191,#7192,#7193,#7194,#7195,#7196,#7197,#7198,#7199,#7200,#7201)),
 .UNSPECIFIED.,.F.,.T.,.F.,(4,4),(4,1,1,1,1,1,1,1,1,1,1,1,1,1,1,1,4),(0.,
1.),(1.5707963267949,2.01959527730772,2.46839422782055,2.91719317833338,
3.36599212884621,3.66519142918809,3.96439072952998,4.26359002987186,4.56278933021375,
5.16118793089752,5.4603872312394,5.75958653158129,6.05878583192317,6.35798513226506,
6.95638373294883,7.40518268346166,7.85398163397448),.UNSPECIFIED.);
#301=B_SPLINE_SURFACE_WITH_KNOTS('',3,3,((#7228,#7229,#7230,#7231,#7232,
#7233,#7234,#7235,#7236,#7237,#7238,#7239,#7240,#7241,#7242,#7243,#7244,
#7245,#7246),(#7247,#7248,#7249,#7250,#7251,#7252,#7253,#7254,#7255,#7256,
#7257,#7258,#7259,#7260,#7261,#7262,#7263,#7264,#7265),(#7266,#7267,#7268,
#7269,#7270,#7271,#7272,#7273,#7274,#7275,#7276,#7277,#7278,#7279,#7280,
#7281,#7282,#7283,#7284),(#7285,#7286,#7287,#7288,#7289,#7290,#7291,#7292,
#7293,#7294,#7295,#7296,#7297,#7298,#7299,#7300,#7301,#7302,#7303)),
 .UNSPECIFIED.,.F.,.T.,.F.,(4,4),(4,1,1,1,1,1,1,1,1,1,1,1,1,1,1,1,4),(0.,
1.),(1.5707963267949,2.01959527730772,2.46839422782055,2.91719317833338,
3.36599212884621,3.66519142918809,3.96439072952998,4.26359002987186,4.56278933021375,
5.16118793089752,5.4603872312394,5.75958653158129,6.05878583192317,6.35798513226506,
6.95638373294883,7.40518268346166,7.85398163397448),.UNSPECIFIED.);
#302=B_SPLINE_SURFACE_WITH_KNOTS('',3,3,((#7382,#7383,#7384,#7385,#7386),
(#7387,#7388,#7389,#7390,#7391),(#7392,#7393,#7394,#7395,#7396),(#7397,
#7398,#7399,#7400,#7401),(#7402,#7403,#7404,#7405,#7406)),.UNSPECIFIED.,
 .F.,.F.,.F.,(4,1,4),(4,1,4),(0.,0.5,1.),(0.,0.00785862436681818,0.0157172487336364),
 .UNSPECIFIED.);
#303=B_SPLINE_SURFACE_WITH_KNOTS('',3,3,((#7426,#7427,#7428,#7429,#7430),
(#7431,#7432,#7433,#7434,#7435),(#7436,#7437,#7438,#7439,#7440),(#7441,
#7442,#7443,#7444,#7445),(#7446,#7447,#7448,#7449,#7450)),.UNSPECIFIED.,
 .F.,.F.,.F.,(4,1,4),(4,1,4),(0.,0.5,1.),(0.,0.00785894990202256,0.0157178998040451),
 .UNSPECIFIED.);
#304=B_SPLINE_SURFACE_WITH_KNOTS('',3,3,((#7510,#7511,#7512,#7513,#7514),
(#7515,#7516,#7517,#7518,#7519),(#7520,#7521,#7522,#7523,#7524),(#7525,
#7526,#7527,#7528,#7529),(#7530,#7531,#7532,#7533,#7534)),.UNSPECIFIED.,
 .F.,.F.,.F.,(4,1,4),(4,1,4),(0.,0.5,1.),(1.02053899928999E-18,0.00785895027235015,
0.0157179005447003),.UNSPECIFIED.);
#305=B_SPLINE_SURFACE_WITH_KNOTS('',3,3,((#7554,#7555,#7556,#7557,#7558),
(#7559,#7560,#7561,#7562,#7563),(#7564,#7565,#7566,#7567,#7568),(#7569,
#7570,#7571,#7572,#7573),(#7574,#7575,#7576,#7577,#7578)),.UNSPECIFIED.,
 .F.,.F.,.F.,(4,1,4),(4,1,4),(0.,0.5,1.),(0.,0.00785862401697905,0.0157172480339581),
 .UNSPECIFIED.);
#306=B_SPLINE_SURFACE_WITH_KNOTS('',3,3,((#9182,#9183,#9184,#9185,#9186,
#9187,#9188,#9189,#9190,#9191,#9192,#9193,#9194,#9195,#9196,#9197,#9198,
#9199,#9200,#9201,#9202,#9203,#9204,#9205,#9206,#9207,#9208,#9209,#9210,
#9211,#9212,#9213,#9214,#9215,#9216,#9217,#9218,#9219,#9220,#9221,#9222,
#9223,#9224,#9225,#9226,#9227,#9228,#9229,#9230,#9231,#9232,#9233,#9234,
#9235,#9236,#9237,#9238,#9239,#9240,#9241,#9242,#9243,#9244,#9245,#9246,
#9247,#9248,#9249,#9250,#9251,#9252,#9253,#9254,#9255,#9256,#9257,#9258,
#9259,#9260,#9261,#9262,#9263,#9264,#9265,#9266,#9267,#9268,#9269,#9270,
#9271,#9272,#9273,#9274,#9275,#9276,#9277,#9278,#9279,#9280,#9281,#9282,
#9283,#9284,#9285,#9286,#9287,#9288,#9289,#9290,#9291,#9292,#9293,#9294,
#9295,#9296),(#9297,#9298,#9299,#9300,#9301,#9302,#9303,#9304,#9305,#9306,
#9307,#9308,#9309,#9310,#9311,#9312,#9313,#9314,#9315,#9316,#9317,#9318,
#9319,#9320,#9321,#9322,#9323,#9324,#9325,#9326,#9327,#9328,#9329,#9330,
#9331,#9332,#9333,#9334,#9335,#9336,#9337,#9338,#9339,#9340,#9341,#9342,
#9343,#9344,#9345,#9346,#9347,#9348,#9349,#9350,#9351,#9352,#9353,#9354,
#9355,#9356,#9357,#9358,#9359,#9360,#9361,#9362,#9363,#9364,#9365,#9366,
#9367,#9368,#9369,#9370,#9371,#9372,#9373,#9374,#9375,#9376,#9377,#9378,
#9379,#9380,#9381,#9382,#9383,#9384,#9385,#9386,#9387,#9388,#9389,#9390,
#9391,#9392,#9393,#9394,#9395,#9396,#9397,#9398,#9399,#9400,#9401,#9402,
#9403,#9404,#9405,#9406,#9407,#9408,#9409,#9410,#9411),(#9412,#9413,#9414,
#9415,#9416,#9417,#9418,#9419,#9420,#9421,#9422,#9423,#9424,#9425,#9426,
#9427,#9428,#9429,#9430,#9431,#9432,#9433,#9434,#9435,#9436,#9437,#9438,
#9439,#9440,#9441,#9442,#9443,#9444,#9445,#9446,#9447,#9448,#9449,#9450,
#9451,#9452,#9453,#9454,#9455,#9456,#9457,#9458,#9459,#9460,#9461,#9462,
#9463,#9464,#9465,#9466,#9467,#9468,#9469,#9470,#9471,#9472,#9473,#9474,
#9475,#9476,#9477,#9478,#9479,#9480,#9481,#9482,#9483,#9484,#9485,#9486,
#9487,#9488,#9489,#9490,#9491,#9492,#9493,#9494,#9495,#9496,#9497,#9498,
#9499,#9500,#9501,#9502,#9503,#9504,#9505,#9506,#9507,#9508,#9509,#9510,
#9511,#9512,#9513,#9514,#9515,#9516,#9517,#9518,#9519,#9520,#9521,#9522,
#9523,#9524,#9525,#9526),(#9527,#9528,#9529,#9530,#9531,#9532,#9533,#9534,
#9535,#9536,#9537,#9538,#9539,#9540,#9541,#9542,#9543,#9544,#9545,#9546,
#9547,#9548,#9549,#9550,#9551,#9552,#9553,#9554,#9555,#9556,#9557,#9558,
#9559,#9560,#9561,#9562,#9563,#9564,#9565,#9566,#9567,#9568,#9569,#9570,
#9571,#9572,#9573,#9574,#9575,#9576,#9577,#9578,#9579,#9580,#9581,#9582,
#9583,#9584,#9585,#9586,#9587,#9588,#9589,#9590,#9591,#9592,#9593,#9594,
#9595,#9596,#9597,#9598,#9599,#9600,#9601,#9602,#9603,#9604,#9605,#9606,
#9607,#9608,#9609,#9610,#9611,#9612,#9613,#9614,#9615,#9616,#9617,#9618,
#9619,#9620,#9621,#9622,#9623,#9624,#9625,#9626,#9627,#9628,#9629,#9630,
#9631,#9632,#9633,#9634,#9635,#9636,#9637,#9638,#9639,#9640,#9641)),
 .UNSPECIFIED.,.F.,.F.,.F.,(4,4),(4,1,1,1,1,1,1,1,1,1,1,1,1,1,1,1,1,1,1,
1,1,1,1,1,1,1,1,1,1,1,1,1,1,1,1,1,1,1,1,1,1,1,1,1,1,1,1,1,1,1,1,1,1,1,1,
1,1,1,1,1,1,1,1,1,1,1,1,1,1,1,1,1,1,1,1,1,1,1,1,1,1,1,1,1,1,1,1,1,1,1,1,
1,1,1,1,1,1,1,1,1,1,1,1,1,1,1,1,1,1,1,1,1,4),(0.,0.0593920221915367),(11.8785778954414,
12.8729398037614,13.8673017120813,14.8616636204013,15.8560255287213,16.8503874370412,
17.8447493453612,18.8391112536811,19.8334731620011,20.8278350703211,21.822196978641,
22.816558886961,23.810920795281,24.8052827036009,25.7996446119209,26.7940065202408,
27.7883684285608,28.7827303368808,29.7770922452007,30.7714541535207,31.7658160618407,
32.7601779701606,33.7545398784806,34.7489017868006,35.7432636951205,36.7376256034405,
37.7319875117605,38.7263494200804,39.7207113284004,40.7150732367203,41.7094351450403,
42.7037970533603,43.6981589616802,44.6925208700002,45.6868827783202,46.6812446866401,
47.6756065949601,48.6699685032801,49.6643304116,50.65869231992,51.6530542282399,
52.6474161365599,53.6417780448799,54.6361399531998,55.6305018615198,56.6248637698398,
57.6192256781597,58.6135875864797,59.6079494947996,60.6023114031196,61.5966733114396,
62.5910352197595,63.5853971280795,64.5797590363995,65.5741209447194,66.5684828530394,
67.5628447613594,68.5572066696793,69.5515685779993,70.5459304863193,71.5402923946392,
72.5346543029592,73.5290162112791,74.5233781195991,75.5177400279191,76.512101936239,
77.506463844559,78.500825752879,79.4951876611989,80.4895495695189,81.4839114778388,
82.4782733861588,83.4726352944788,84.4669972027987,85.4613591111187,86.4557210194387,
87.4500829277586,88.4444448360786,89.4388067443986,90.4331686527185,91.4275305610385,
92.4218924693585,93.4162543776784,94.4106162859984,95.4049781943183,96.3993401026383,
97.3937020109583,98.3880639192782,99.3824258275982,100.376787735918,101.371149644238,
102.365511552558,103.359873460878,104.354235369198,105.348597277518,106.342959185838,
107.337321094158,108.331683002478,109.326044910798,110.320406819118,111.314768727438,
112.309130635758,113.303492544078,114.297854452398,115.292216360718,116.286578269038,
117.280940177358,118.275302085678,119.269663993997,120.264025902317,121.258387810637,
122.252749718957,123.247111627277),.UNSPECIFIED.);
#307=B_SPLINE_SURFACE_WITH_KNOTS('',3,3,((#9835,#9836,#9837,#9838,#9839,
#9840,#9841,#9842,#9843,#9844,#9845,#9846,#9847,#9848,#9849,#9850,#9851,
#9852,#9853,#9854,#9855,#9856,#9857,#9858,#9859,#9860,#9861,#9862,#9863,
#9864,#9865,#9866,#9867,#9868,#9869,#9870,#9871,#9872,#9873,#9874,#9875,
#9876,#9877,#9878,#9879,#9880,#9881,#9882,#9883,#9884,#9885,#9886,#9887,
#9888,#9889,#9890,#9891,#9892,#9893,#9894,#9895,#9896,#9897,#9898,#9899,
#9900,#9901,#9902,#9903,#9904,#9905,#9906,#9907,#9908,#9909,#9910,#9911,
#9912,#9913,#9914,#9915,#9916,#9917,#9918,#9919,#9920,#9921,#9922,#9923,
#9924,#9925,#9926,#9927,#9928,#9929,#9930,#9931,#9932,#9933,#9934,#9935,
#9936,#9937,#9938,#9939,#9940,#9941,#9942,#9943,#9944,#9945,#9946,#9947,
#9948,#9949),(#9950,#9951,#9952,#9953,#9954,#9955,#9956,#9957,#9958,#9959,
#9960,#9961,#9962,#9963,#9964,#9965,#9966,#9967,#9968,#9969,#9970,#9971,
#9972,#9973,#9974,#9975,#9976,#9977,#9978,#9979,#9980,#9981,#9982,#9983,
#9984,#9985,#9986,#9987,#9988,#9989,#9990,#9991,#9992,#9993,#9994,#9995,
#9996,#9997,#9998,#9999,#10000,#10001,#10002,#10003,#10004,#10005,#10006,
#10007,#10008,#10009,#10010,#10011,#10012,#10013,#10014,#10015,#10016,#10017,
#10018,#10019,#10020,#10021,#10022,#10023,#10024,#10025,#10026,#10027,#10028,
#10029,#10030,#10031,#10032,#10033,#10034,#10035,#10036,#10037,#10038,#10039,
#10040,#10041,#10042,#10043,#10044,#10045,#10046,#10047,#10048,#10049,#10050,
#10051,#10052,#10053,#10054,#10055,#10056,#10057,#10058,#10059,#10060,#10061,
#10062,#10063,#10064),(#10065,#10066,#10067,#10068,#10069,#10070,#10071,
#10072,#10073,#10074,#10075,#10076,#10077,#10078,#10079,#10080,#10081,#10082,
#10083,#10084,#10085,#10086,#10087,#10088,#10089,#10090,#10091,#10092,#10093,
#10094,#10095,#10096,#10097,#10098,#10099,#10100,#10101,#10102,#10103,#10104,
#10105,#10106,#10107,#10108,#10109,#10110,#10111,#10112,#10113,#10114,#10115,
#10116,#10117,#10118,#10119,#10120,#10121,#10122,#10123,#10124,#10125,#10126,
#10127,#10128,#10129,#10130,#10131,#10132,#10133,#10134,#10135,#10136,#10137,
#10138,#10139,#10140,#10141,#10142,#10143,#10144,#10145,#10146,#10147,#10148,
#10149,#10150,#10151,#10152,#10153,#10154,#10155,#10156,#10157,#10158,#10159,
#10160,#10161,#10162,#10163,#10164,#10165,#10166,#10167,#10168,#10169,#10170,
#10171,#10172,#10173,#10174,#10175,#10176,#10177,#10178,#10179),(#10180,
#10181,#10182,#10183,#10184,#10185,#10186,#10187,#10188,#10189,#10190,#10191,
#10192,#10193,#10194,#10195,#10196,#10197,#10198,#10199,#10200,#10201,#10202,
#10203,#10204,#10205,#10206,#10207,#10208,#10209,#10210,#10211,#10212,#10213,
#10214,#10215,#10216,#10217,#10218,#10219,#10220,#10221,#10222,#10223,#10224,
#10225,#10226,#10227,#10228,#10229,#10230,#10231,#10232,#10233,#10234,#10235,
#10236,#10237,#10238,#10239,#10240,#10241,#10242,#10243,#10244,#10245,#10246,
#10247,#10248,#10249,#10250,#10251,#10252,#10253,#10254,#10255,#10256,#10257,
#10258,#10259,#10260,#10261,#10262,#10263,#10264,#10265,#10266,#10267,#10268,
#10269,#10270,#10271,#10272,#10273,#10274,#10275,#10276,#10277,#10278,#10279,
#10280,#10281,#10282,#10283,#10284,#10285,#10286,#10287,#10288,#10289,#10290,
#10291,#10292,#10293,#10294)),.UNSPECIFIED.,.F.,.F.,.F.,(4,4),(4,1,1,1,
1,1,1,1,1,1,1,1,1,1,1,1,1,1,1,1,1,1,1,1,1,1,1,1,1,1,1,1,1,1,1,1,1,1,1,1,
1,1,1,1,1,1,1,1,1,1,1,1,1,1,1,1,1,1,1,1,1,1,1,1,1,1,1,1,1,1,1,1,1,1,1,1,
1,1,1,1,1,1,1,1,1,1,1,1,1,1,1,1,1,1,1,1,1,1,1,1,1,1,1,1,1,1,1,1,1,1,1,1,
4),(0.,0.0593920221915367),(14.6327430048308,15.6271049131507,16.6214668214707,
17.6158287297907,18.6101906381106,19.6045525464306,20.5989144547506,21.5932763630705,
22.5876382713905,23.5820001797105,24.5763620880304,25.5707239963504,26.5650859046703,
27.5594478129903,28.5538097213103,29.5481716296302,30.5425335379502,31.5368954462702,
32.5312573545901,33.5256192629101,34.5199811712301,35.51434307955,36.50870498787,
37.5030668961899,38.4974288045099,39.4917907128299,40.4861526211498,41.4805145294698,
42.4748764377898,43.4692383461097,44.4636002544297,45.4579621627497,46.4523240710696,
47.4466859793896,48.4410478877095,49.4354097960295,50.4297717043495,51.4241336126694,
52.4184955209894,53.4128574293094,54.4072193376293,55.4015812459493,56.3959431542693,
57.3903050625892,58.3846669709092,59.3790288792291,60.3733907875491,61.3677526958691,
62.362114604189,63.356476512509,64.350838420829,65.3452003291489,66.3395622374689,
67.3339241457888,68.3282860541088,69.3226479624288,70.3170098707487,71.3113717790687,
72.3057336873887,73.3000955957086,74.2944575040286,75.2888194123486,76.2831813206685,
77.2775432289885,78.2719051373085,79.2662670456284,80.2606289539484,81.2549908622683,
82.2493527705883,83.2437146789083,84.2380765872282,85.2324384955482,86.2268004038682,
87.2211623121881,88.2155242205081,89.209886128828,90.204248037148,91.198609945468,
92.1929718537879,93.1873337621079,94.1816956704279,95.1760575787478,96.1704194870678,
97.1647813953878,98.1591433037077,99.1535052120277,100.147867120348,101.142229028668,
102.136590936988,103.130952845308,104.125314753628,105.119676661947,106.114038570267,
107.108400478587,108.102762386907,109.097124295227,110.091486203547,111.085848111867,
112.080210020187,113.074571928507,114.068933836827,115.063295745147,116.057657653467,
117.052019561787,118.046381470107,119.040743378427,120.035105286747,121.029467195067,
122.023829103387,123.018191011707,124.012552920027,125.006914828347,126.001276736667),
 .UNSPECIFIED.);
#308=B_SPLINE_SURFACE_WITH_KNOTS('',3,3,((#10445,#10446,#10447,#10448),
(#10449,#10450,#10451,#10452),(#10453,#10454,#10455,#10456),(#10457,#10458,
#10459,#10460),(#10461,#10462,#10463,#10464)),.UNSPECIFIED.,.F.,.F.,.F.,
(4,1,4),(4,4),(0.,0.5,1.),(0.088693979487329,0.125274232772668),
 .UNSPECIFIED.);
#309=B_SPLINE_SURFACE_WITH_KNOTS('',3,3,((#10506,#10507,#10508,#10509,#10510,
#10511,#10512,#10513,#10514,#10515,#10516,#10517,#10518,#10519,#10520,#10521,
#10522,#10523,#10524,#10525,#10526,#10527),(#10528,#10529,#10530,#10531,
#10532,#10533,#10534,#10535,#10536,#10537,#10538,#10539,#10540,#10541,#10542,
#10543,#10544,#10545,#10546,#10547,#10548,#10549),(#10550,#10551,#10552,
#10553,#10554,#10555,#10556,#10557,#10558,#10559,#10560,#10561,#10562,#10563,
#10564,#10565,#10566,#10567,#10568,#10569,#10570,#10571),(#10572,#10573,
#10574,#10575,#10576,#10577,#10578,#10579,#10580,#10581,#10582,#10583,#10584,
#10585,#10586,#10587,#10588,#10589,#10590,#10591,#10592,#10593)),
 .UNSPECIFIED.,.F.,.F.,.F.,(4,4),(4,1,1,1,1,1,1,1,1,1,1,1,1,1,1,1,1,1,1,
4),(0.,1.),(0.,2.49089996579439,4.98179993158877,6.64239990878503,8.30299988598129,
9.96359986317755,11.6241998403738,13.2847998175701,14.9453997947663,16.6059997719626,
18.2665997491588,19.9271997263551,21.5877997035514,23.2483996807476,24.9089996579439,
26.5695996351401,28.2301996123364,29.8907995895326,32.381699555327,34.8725995211214),
 .UNSPECIFIED.);
#310=B_SPLINE_SURFACE_WITH_KNOTS('',3,3,((#10649,#10650,#10651,#10652),
(#10653,#10654,#10655,#10656),(#10657,#10658,#10659,#10660),(#10661,#10662,
#10663,#10664),(#10665,#10666,#10667,#10668)),.UNSPECIFIED.,.F.,.F.,.F.,
(4,1,4),(4,4),(0.,0.5,1.),(0.0886939794873267,0.125274232772633),
 .UNSPECIFIED.);
#311=B_SPLINE_SURFACE_WITH_KNOTS('',3,3,((#10677,#10678,#10679,#10680),
(#10681,#10682,#10683,#10684),(#10685,#10686,#10687,#10688),(#10689,#10690,
#10691,#10692)),.UNSPECIFIED.,.F.,.F.,.F.,(4,4),(4,4),(0.,1.),(0.587131769179142,
0.860462555942468),.UNSPECIFIED.);
#312=B_SPLINE_SURFACE_WITH_KNOTS('',3,3,((#10968,#10969,#10970,#10971),
(#10972,#10973,#10974,#10975),(#10976,#10977,#10978,#10979),(#10980,#10981,
#10982,#10983)),.UNSPECIFIED.,.F.,.F.,.F.,(4,4),(4,4),(0.,1.),(0.0190073922957582,
0.292336438831091),.UNSPECIFIED.);
#313=B_SPLINE_SURFACE_WITH_KNOTS('',3,3,((#11013,#11014,#11015,#11016,#11017,
#11018,#11019,#11020,#11021,#11022,#11023,#11024,#11025,#11026,#11027,#11028,
#11029,#11030,#11031,#11032,#11033,#11034,#11035),(#11036,#11037,#11038,
#11039,#11040,#11041,#11042,#11043,#11044,#11045,#11046,#11047,#11048,#11049,
#11050,#11051,#11052,#11053,#11054,#11055,#11056,#11057,#11058),(#11059,
#11060,#11061,#11062,#11063,#11064,#11065,#11066,#11067,#11068,#11069,#11070,
#11071,#11072,#11073,#11074,#11075,#11076,#11077,#11078,#11079,#11080,#11081),
(#11082,#11083,#11084,#11085,#11086,#11087,#11088,#11089,#11090,#11091,
#11092,#11093,#11094,#11095,#11096,#11097,#11098,#11099,#11100,#11101,#11102,
#11103,#11104)),.UNSPECIFIED.,.F.,.T.,.F.,(4,4),(4,1,1,1,1,1,1,1,1,1,1,
1,1,1,1,1,1,1,1,1,4),(0.,1.),(1.5707963267949,2.01959527730772,2.46839422782055,
2.76759352816244,3.06679282850432,3.36599212884621,3.66519142918809,3.96439072952998,
4.26359002987186,4.56278933021375,4.86198863055563,5.16118793089752,5.4603872312394,
5.75958653158129,6.05878583192317,6.20838548209412,6.35798513226506,6.65718443260694,
6.95638373294883,7.40518268346166,7.85398163397448),.UNSPECIFIED.);
#314=B_SPLINE_SURFACE_WITH_KNOTS('',3,3,((#11243,#11244,#11245,#11246,#11247,
#11248,#11249,#11250,#11251,#11252,#11253,#11254,#11255,#11256,#11257,#11258,
#11259,#11260,#11261,#11262,#11263),(#11264,#11265,#11266,#11267,#11268,
#11269,#11270,#11271,#11272,#11273,#11274,#11275,#11276,#11277,#11278,#11279,
#11280,#11281,#11282,#11283,#11284),(#11285,#11286,#11287,#11288,#11289,
#11290,#11291,#11292,#11293,#11294,#11295,#11296,#11297,#11298,#11299,#11300,
#11301,#11302,#11303,#11304,#11305),(#11306,#11307,#11308,#11309,#11310,
#11311,#11312,#11313,#11314,#11315,#11316,#11317,#11318,#11319,#11320,#11321,
#11322,#11323,#11324,#11325,#11326),(#11327,#11328,#11329,#11330,#11331,
#11332,#11333,#11334,#11335,#11336,#11337,#11338,#11339,#11340,#11341,#11342,
#11343,#11344,#11345,#11346,#11347)),.UNSPECIFIED.,.F.,.F.,.F.,(4,1,4),
(4,1,1,1,1,1,1,1,1,1,1,1,1,1,1,1,1,1,4),(0.,0.5,1.),(0.,2.5201892997592,
5.0403785995184,6.72050479935786,8.40063099919733,10.0807571990368,11.7608833988763,
15.1211357985552,15.9611988984749,16.8012619983947,20.1615143980736,21.841640597913,
23.5217667977525,25.201892997592,26.8820191974314,28.5621453972709,30.2422715971104,
32.7624608968696,35.2826501966288),.UNSPECIFIED.);
#315=B_SPLINE_SURFACE_WITH_KNOTS('',3,3,((#11381,#11382,#11383,#11384),
(#11385,#11386,#11387,#11388),(#11389,#11390,#11391,#11392),(#11393,#11394,
#11395,#11396)),.UNSPECIFIED.,.F.,.F.,.F.,(4,4),(4,4),(0.,1.),(0.825569897711632,
1.1096475233552),.UNSPECIFIED.);
#316=B_SPLINE_SURFACE_WITH_KNOTS('',3,3,((#11679,#11680,#11681,#11682),
(#11683,#11684,#11685,#11686),(#11687,#11688,#11689,#11690),(#11691,#11692,
#11693,#11694)),.UNSPECIFIED.,.F.,.F.,.F.,(4,4),(4,4),(0.,1.),(0.0332835073847237,
0.317361133028268),.UNSPECIFIED.);
#317=B_SPLINE_SURFACE_WITH_KNOTS('',3,3,((#11721,#11722,#11723,#11724),
(#11725,#11726,#11727,#11728),(#11729,#11730,#11731,#11732),(#11733,#11734,
#11735,#11736)),.UNSPECIFIED.,.F.,.F.,.F.,(4,4),(4,4),(0.,1.),(34.6574150541607,
35.1575805274809),.UNSPECIFIED.);
#318=B_SPLINE_SURFACE_WITH_KNOTS('',3,3,((#11766,#11767,#11768,#11769),
(#11770,#11771,#11772,#11773),(#11774,#11775,#11776,#11777),(#11778,#11779,
#11780,#11781),(#11782,#11783,#11784,#11785)),.UNSPECIFIED.,.F.,.F.,.F.,
(4,1,4),(4,4),(0.,0.5,1.),(35.8573857487427,36.3575403182),
 .UNSPECIFIED.);
#319=B_SPLINE_SURFACE_WITH_KNOTS('',3,3,((#11947,#11948,#11949,#11950,#11951,
#11952,#11953,#11954,#11955,#11956,#11957,#11958,#11959),(#11960,#11961,
#11962,#11963,#11964,#11965,#11966,#11967,#11968,#11969,#11970,#11971,#11972),
(#11973,#11974,#11975,#11976,#11977,#11978,#11979,#11980,#11981,#11982,
#11983,#11984,#11985),(#11986,#11987,#11988,#11989,#11990,#11991,#11992,
#11993,#11994,#11995,#11996,#11997,#11998),(#11999,#12000,#12001,#12002,
#12003,#12004,#12005,#12006,#12007,#12008,#12009,#12010,#12011),(#12012,
#12013,#12014,#12015,#12016,#12017,#12018,#12019,#12020,#12021,#12022,#12023,
#12024),(#12025,#12026,#12027,#12028,#12029,#12030,#12031,#12032,#12033,
#12034,#12035,#12036,#12037)),.UNSPECIFIED.,.F.,.F.,.F.,(4,1,1,1,4),(4,
1,1,1,1,1,1,1,1,1,4),(0.,0.285714285714286,0.571428571428571,0.785714285714286,
1.),(-0.510305664677257,-0.435654171543958,-0.361002678410658,-0.323676931844009,
-0.305014058560684,-0.286351185277359,-0.267688311994034,-0.211699692144059,
-0.13704819901076,-0.0623967058774603,0.0122547872558393),.UNSPECIFIED.);
#320=B_SPLINE_SURFACE_WITH_KNOTS('',3,3,((#12242,#12243,#12244,#12245),
(#12246,#12247,#12248,#12249),(#12250,#12251,#12252,#12253),(#12254,#12255,
#12256,#12257),(#12258,#12259,#12260,#12261),(#12262,#12263,#12264,#12265)),
 .UNSPECIFIED.,.F.,.F.,.F.,(4,1,1,4),(4,4),(0.,0.285714285714286,0.571428571428571,
1.),(0.,0.0695988259914621),.UNSPECIFIED.);
#321=B_SPLINE_SURFACE_WITH_KNOTS('',3,3,((#12295,#12296,#12297,#12298),
(#12299,#12300,#12301,#12302),(#12303,#12304,#12305,#12306),(#12307,#12308,
#12309,#12310),(#12311,#12312,#12313,#12314)),.UNSPECIFIED.,.F.,.F.,.F.,
(4,1,4),(4,4),(0.248288368736695,0.460547516100694,0.743559712586026),(1.50567154478811,
1.5257178645514),.UNSPECIFIED.);
#322=B_SPLINE_SURFACE_WITH_KNOTS('',3,3,((#12315,#12316,#12317,#12318),
(#12319,#12320,#12321,#12322),(#12323,#12324,#12325,#12326),(#12327,#12328,
#12329,#12330),(#12331,#12332,#12333,#12334)),.UNSPECIFIED.,.F.,.F.,.F.,
(4,1,4),(4,4),(0.248288368736683,0.460547516100081,0.743559712584612),(0.999225034210935,
1.01926765266779),.UNSPECIFIED.);
#323=B_SPLINE_SURFACE_WITH_KNOTS('',3,3,((#12395,#12396,#12397,#12398),
(#12399,#12400,#12401,#12402),(#12403,#12404,#12405,#12406),(#12407,#12408,
#12409,#12410),(#12411,#12412,#12413,#12414),(#12415,#12416,#12417,#12418)),
 .UNSPECIFIED.,.F.,.F.,.F.,(4,1,1,4),(4,4),(0.,0.285714285714286,0.571428571428571,
1.),(0.096109917502246,0.165708743493706),.UNSPECIFIED.);
#324=FACE_OUTER_BOUND('',#594,.T.);
#325=FACE_OUTER_BOUND('',#595,.T.);
#326=FACE_OUTER_BOUND('',#596,.T.);
#327=FACE_OUTER_BOUND('',#597,.T.);
#328=FACE_OUTER_BOUND('',#598,.T.);
#329=FACE_OUTER_BOUND('',#600,.T.);
#330=FACE_OUTER_BOUND('',#601,.T.);
#331=FACE_OUTER_BOUND('',#602,.T.);
#332=FACE_OUTER_BOUND('',#603,.T.);
#333=FACE_OUTER_BOUND('',#605,.T.);
#334=FACE_OUTER_BOUND('',#606,.T.);
#335=FACE_OUTER_BOUND('',#608,.T.);
#336=FACE_OUTER_BOUND('',#609,.T.);
#337=FACE_OUTER_BOUND('',#610,.T.);
#338=FACE_OUTER_BOUND('',#611,.T.);
#339=FACE_OUTER_BOUND('',#612,.T.);
#340=FACE_OUTER_BOUND('',#613,.T.);
#341=FACE_OUTER_BOUND('',#614,.T.);
#342=FACE_OUTER_BOUND('',#615,.T.);
#343=FACE_OUTER_BOUND('',#616,.T.);
#344=FACE_OUTER_BOUND('',#617,.T.);
#345=FACE_OUTER_BOUND('',#618,.T.);
#346=FACE_OUTER_BOUND('',#619,.T.);
#347=FACE_OUTER_BOUND('',#620,.T.);
#348=FACE_OUTER_BOUND('',#621,.T.);
#349=FACE_OUTER_BOUND('',#622,.T.);
#350=FACE_OUTER_BOUND('',#623,.T.);
#351=FACE_OUTER_BOUND('',#624,.T.);
#352=FACE_OUTER_BOUND('',#625,.T.);
#353=FACE_OUTER_BOUND('',#626,.T.);
#354=FACE_OUTER_BOUND('',#627,.T.);
#355=FACE_OUTER_BOUND('',#628,.T.);
#356=FACE_OUTER_BOUND('',#629,.T.);
#357=FACE_OUTER_BOUND('',#630,.T.);
#358=FACE_OUTER_BOUND('',#631,.T.);
#359=FACE_OUTER_BOUND('',#633,.T.);
#360=FACE_OUTER_BOUND('',#634,.T.);
#361=FACE_OUTER_BOUND('',#635,.T.);
#362=FACE_OUTER_BOUND('',#636,.T.);
#363=FACE_OUTER_BOUND('',#637,.T.);
#364=FACE_OUTER_BOUND('',#638,.T.);
#365=FACE_OUTER_BOUND('',#639,.T.);
#366=FACE_OUTER_BOUND('',#640,.T.);
#367=FACE_OUTER_BOUND('',#641,.T.);
#368=FACE_OUTER_BOUND('',#642,.T.);
#369=FACE_OUTER_BOUND('',#644,.T.);
#370=FACE_OUTER_BOUND('',#645,.T.);
#371=FACE_OUTER_BOUND('',#646,.T.);
#372=FACE_OUTER_BOUND('',#647,.T.);
#373=FACE_OUTER_BOUND('',#648,.T.);
#374=FACE_OUTER_BOUND('',#649,.T.);
#375=FACE_OUTER_BOUND('',#650,.T.);
#376=FACE_OUTER_BOUND('',#651,.T.);
#377=FACE_OUTER_BOUND('',#652,.T.);
#378=FACE_OUTER_BOUND('',#653,.T.);
#379=FACE_OUTER_BOUND('',#654,.T.);
#380=FACE_OUTER_BOUND('',#655,.T.);
#381=FACE_OUTER_BOUND('',#656,.T.);
#382=FACE_OUTER_BOUND('',#657,.T.);
#383=FACE_OUTER_BOUND('',#658,.T.);
#384=FACE_OUTER_BOUND('',#659,.T.);
#385=FACE_OUTER_BOUND('',#660,.T.);
#386=FACE_OUTER_BOUND('',#661,.T.);
#387=FACE_OUTER_BOUND('',#662,.T.);
#388=FACE_OUTER_BOUND('',#663,.T.);
#389=FACE_OUTER_BOUND('',#664,.T.);
#390=FACE_OUTER_BOUND('',#665,.T.);
#391=FACE_OUTER_BOUND('',#666,.T.);
#392=FACE_OUTER_BOUND('',#667,.T.);
#393=FACE_OUTER_BOUND('',#668,.T.);
#394=FACE_OUTER_BOUND('',#669,.T.);
#395=FACE_OUTER_BOUND('',#670,.T.);
#396=FACE_OUTER_BOUND('',#671,.T.);
#397=FACE_OUTER_BOUND('',#672,.T.);
#398=FACE_OUTER_BOUND('',#673,.T.);
#399=FACE_OUTER_BOUND('',#674,.T.);
#400=FACE_OUTER_BOUND('',#675,.T.);
#401=FACE_OUTER_BOUND('',#676,.T.);
#402=FACE_OUTER_BOUND('',#677,.T.);
#403=FACE_OUTER_BOUND('',#678,.T.);
#404=FACE_OUTER_BOUND('',#679,.T.);
#405=FACE_OUTER_BOUND('',#680,.T.);
#406=FACE_OUTER_BOUND('',#681,.T.);
#407=FACE_OUTER_BOUND('',#682,.T.);
#408=FACE_OUTER_BOUND('',#683,.T.);
#409=FACE_OUTER_BOUND('',#684,.T.);
#410=FACE_OUTER_BOUND('',#685,.T.);
#411=FACE_OUTER_BOUND('',#686,.T.);
#412=FACE_OUTER_BOUND('',#687,.T.);
#413=FACE_OUTER_BOUND('',#688,.T.);
#414=FACE_OUTER_BOUND('',#689,.T.);
#415=FACE_OUTER_BOUND('',#690,.T.);
#416=FACE_OUTER_BOUND('',#691,.T.);
#417=FACE_OUTER_BOUND('',#692,.T.);
#418=FACE_OUTER_BOUND('',#693,.T.);
#419=FACE_OUTER_BOUND('',#694,.T.);
#420=FACE_OUTER_BOUND('',#695,.T.);
#421=FACE_OUTER_BOUND('',#696,.T.);
#422=FACE_OUTER_BOUND('',#697,.T.);
#423=FACE_OUTER_BOUND('',#698,.T.);
#424=FACE_OUTER_BOUND('',#699,.T.);
#425=FACE_OUTER_BOUND('',#700,.T.);
#426=FACE_OUTER_BOUND('',#702,.T.);
#427=FACE_OUTER_BOUND('',#703,.T.);
#428=FACE_OUTER_BOUND('',#705,.T.);
#429=FACE_OUTER_BOUND('',#708,.T.);
#430=FACE_OUTER_BOUND('',#710,.T.);
#431=FACE_OUTER_BOUND('',#711,.T.);
#432=FACE_OUTER_BOUND('',#713,.T.);
#433=FACE_OUTER_BOUND('',#714,.T.);
#434=FACE_OUTER_BOUND('',#715,.T.);
#435=FACE_OUTER_BOUND('',#716,.T.);
#436=FACE_OUTER_BOUND('',#717,.T.);
#437=FACE_OUTER_BOUND('',#718,.T.);
#438=FACE_OUTER_BOUND('',#720,.T.);
#439=FACE_OUTER_BOUND('',#721,.T.);
#440=FACE_OUTER_BOUND('',#722,.T.);
#441=FACE_OUTER_BOUND('',#723,.T.);
#442=FACE_OUTER_BOUND('',#724,.T.);
#443=FACE_OUTER_BOUND('',#725,.T.);
#444=FACE_OUTER_BOUND('',#726,.T.);
#445=FACE_OUTER_BOUND('',#727,.T.);
#446=FACE_OUTER_BOUND('',#728,.T.);
#447=FACE_OUTER_BOUND('',#729,.T.);
#448=FACE_OUTER_BOUND('',#730,.T.);
#449=FACE_OUTER_BOUND('',#731,.T.);
#450=FACE_OUTER_BOUND('',#732,.T.);
#451=FACE_OUTER_BOUND('',#733,.T.);
#452=FACE_OUTER_BOUND('',#734,.T.);
#453=FACE_OUTER_BOUND('',#735,.T.);
#454=FACE_OUTER_BOUND('',#736,.T.);
#455=FACE_OUTER_BOUND('',#737,.T.);
#456=FACE_OUTER_BOUND('',#739,.T.);
#457=FACE_OUTER_BOUND('',#740,.T.);
#458=FACE_OUTER_BOUND('',#741,.T.);
#459=FACE_OUTER_BOUND('',#742,.T.);
#460=FACE_OUTER_BOUND('',#743,.T.);
#461=FACE_OUTER_BOUND('',#744,.T.);
#462=FACE_OUTER_BOUND('',#745,.T.);
#463=FACE_OUTER_BOUND('',#746,.T.);
#464=FACE_OUTER_BOUND('',#747,.T.);
#465=FACE_OUTER_BOUND('',#748,.T.);
#466=FACE_OUTER_BOUND('',#749,.T.);
#467=FACE_OUTER_BOUND('',#750,.T.);
#468=FACE_OUTER_BOUND('',#751,.T.);
#469=FACE_OUTER_BOUND('',#752,.T.);
#470=FACE_OUTER_BOUND('',#754,.T.);
#471=FACE_OUTER_BOUND('',#755,.T.);
#472=FACE_OUTER_BOUND('',#756,.T.);
#473=FACE_OUTER_BOUND('',#757,.T.);
#474=FACE_OUTER_BOUND('',#758,.T.);
#475=FACE_OUTER_BOUND('',#759,.T.);
#476=FACE_OUTER_BOUND('',#760,.T.);
#477=FACE_OUTER_BOUND('',#761,.T.);
#478=FACE_OUTER_BOUND('',#762,.T.);
#479=FACE_OUTER_BOUND('',#763,.T.);
#480=FACE_OUTER_BOUND('',#764,.T.);
#481=FACE_OUTER_BOUND('',#765,.T.);
#482=FACE_OUTER_BOUND('',#766,.T.);
#483=FACE_OUTER_BOUND('',#767,.T.);
#484=FACE_OUTER_BOUND('',#768,.T.);
#485=FACE_OUTER_BOUND('',#769,.T.);
#486=FACE_OUTER_BOUND('',#770,.T.);
#487=FACE_OUTER_BOUND('',#771,.T.);
#488=FACE_OUTER_BOUND('',#772,.T.);
#489=FACE_OUTER_BOUND('',#773,.T.);
#490=FACE_OUTER_BOUND('',#775,.T.);
#491=FACE_OUTER_BOUND('',#776,.T.);
#492=FACE_OUTER_BOUND('',#777,.T.);
#493=FACE_OUTER_BOUND('',#778,.T.);
#494=FACE_OUTER_BOUND('',#780,.T.);
#495=FACE_OUTER_BOUND('',#781,.T.);
#496=FACE_OUTER_BOUND('',#783,.T.);
#497=FACE_OUTER_BOUND('',#784,.T.);
#498=FACE_OUTER_BOUND('',#785,.T.);
#499=FACE_OUTER_BOUND('',#786,.T.);
#500=FACE_OUTER_BOUND('',#787,.T.);
#501=FACE_OUTER_BOUND('',#788,.T.);
#502=FACE_OUTER_BOUND('',#789,.T.);
#503=FACE_OUTER_BOUND('',#790,.T.);
#504=FACE_OUTER_BOUND('',#791,.T.);
#505=FACE_OUTER_BOUND('',#792,.T.);
#506=FACE_OUTER_BOUND('',#793,.T.);
#507=FACE_OUTER_BOUND('',#794,.T.);
#508=FACE_OUTER_BOUND('',#795,.T.);
#509=FACE_OUTER_BOUND('',#796,.T.);
#510=FACE_OUTER_BOUND('',#797,.T.);
#511=FACE_OUTER_BOUND('',#798,.T.);
#512=FACE_OUTER_BOUND('',#799,.T.);
#513=FACE_OUTER_BOUND('',#800,.T.);
#514=FACE_OUTER_BOUND('',#801,.T.);
#515=FACE_OUTER_BOUND('',#802,.T.);
#516=FACE_OUTER_BOUND('',#803,.T.);
#517=FACE_OUTER_BOUND('',#804,.T.);
#518=FACE_OUTER_BOUND('',#805,.T.);
#519=FACE_OUTER_BOUND('',#806,.T.);
#520=FACE_OUTER_BOUND('',#807,.T.);
#521=FACE_OUTER_BOUND('',#808,.T.);
#522=FACE_OUTER_BOUND('',#809,.T.);
#523=FACE_OUTER_BOUND('',#810,.T.);
#524=FACE_OUTER_BOUND('',#812,.T.);
#525=FACE_OUTER_BOUND('',#813,.T.);
#526=FACE_OUTER_BOUND('',#814,.T.);
#527=FACE_OUTER_BOUND('',#815,.T.);
#528=FACE_OUTER_BOUND('',#816,.T.);
#529=FACE_OUTER_BOUND('',#817,.T.);
#530=FACE_OUTER_BOUND('',#818,.T.);
#531=FACE_OUTER_BOUND('',#819,.T.);
#532=FACE_OUTER_BOUND('',#820,.T.);
#533=FACE_OUTER_BOUND('',#821,.T.);
#534=FACE_OUTER_BOUND('',#822,.T.);
#535=FACE_OUTER_BOUND('',#823,.T.);
#536=FACE_OUTER_BOUND('',#824,.T.);
#537=FACE_OUTER_BOUND('',#826,.T.);
#538=FACE_OUTER_BOUND('',#827,.T.);
#539=FACE_OUTER_BOUND('',#828,.T.);
#540=FACE_OUTER_BOUND('',#829,.T.);
#541=FACE_OUTER_BOUND('',#831,.T.);
#542=FACE_OUTER_BOUND('',#832,.T.);
#543=FACE_OUTER_BOUND('',#833,.T.);
#544=FACE_OUTER_BOUND('',#834,.T.);
#545=FACE_OUTER_BOUND('',#835,.T.);
#546=FACE_OUTER_BOUND('',#837,.T.);
#547=FACE_OUTER_BOUND('',#838,.T.);
#548=FACE_OUTER_BOUND('',#839,.T.);
#549=FACE_OUTER_BOUND('',#840,.T.);
#550=FACE_OUTER_BOUND('',#842,.T.);
#551=FACE_OUTER_BOUND('',#843,.T.);
#552=FACE_OUTER_BOUND('',#844,.T.);
#553=FACE_OUTER_BOUND('',#845,.T.);
#554=FACE_OUTER_BOUND('',#847,.T.);
#555=FACE_OUTER_BOUND('',#848,.T.);
#556=FACE_OUTER_BOUND('',#850,.T.);
#557=FACE_OUTER_BOUND('',#851,.T.);
#558=FACE_OUTER_BOUND('',#852,.T.);
#559=FACE_OUTER_BOUND('',#855,.T.);
#560=FACE_OUTER_BOUND('',#856,.T.);
#561=FACE_OUTER_BOUND('',#857,.T.);
#562=FACE_OUTER_BOUND('',#858,.T.);
#563=FACE_OUTER_BOUND('',#861,.T.);
#564=FACE_OUTER_BOUND('',#862,.T.);
#565=FACE_OUTER_BOUND('',#863,.T.);
#566=FACE_OUTER_BOUND('',#864,.T.);
#567=FACE_OUTER_BOUND('',#865,.T.);
#568=FACE_OUTER_BOUND('',#866,.T.);
#569=FACE_OUTER_BOUND('',#867,.T.);
#570=FACE_OUTER_BOUND('',#868,.T.);
#571=FACE_OUTER_BOUND('',#869,.T.);
#572=FACE_OUTER_BOUND('',#870,.T.);
#573=FACE_OUTER_BOUND('',#871,.T.);
#574=FACE_OUTER_BOUND('',#872,.T.);
#575=FACE_OUTER_BOUND('',#873,.T.);
#576=FACE_OUTER_BOUND('',#874,.T.);
#577=FACE_OUTER_BOUND('',#875,.T.);
#578=FACE_OUTER_BOUND('',#876,.T.);
#579=FACE_OUTER_BOUND('',#877,.T.);
#580=FACE_OUTER_BOUND('',#878,.T.);
#581=FACE_OUTER_BOUND('',#879,.T.);
#582=FACE_OUTER_BOUND('',#880,.T.);
#583=FACE_OUTER_BOUND('',#881,.T.);
#584=FACE_OUTER_BOUND('',#882,.T.);
#585=FACE_OUTER_BOUND('',#883,.T.);
#586=FACE_OUTER_BOUND('',#884,.T.);
#587=FACE_OUTER_BOUND('',#885,.T.);
#588=FACE_OUTER_BOUND('',#886,.T.);
#589=FACE_OUTER_BOUND('',#887,.T.);
#590=FACE_OUTER_BOUND('',#888,.T.);
#591=FACE_OUTER_BOUND('',#889,.T.);
#592=FACE_OUTER_BOUND('',#890,.T.);
#593=FACE_OUTER_BOUND('',#891,.T.);
#594=EDGE_LOOP('',(#2767,#2768,#2769,#2770,#2771,#2772));
#595=EDGE_LOOP('',(#2773,#2774,#2775,#2776,#2777));
#596=EDGE_LOOP('',(#2778,#2779,#2780,#2781));
#597=EDGE_LOOP('',(#2782,#2783,#2784,#2785,#2786));
#598=EDGE_LOOP('',(#2787));
#599=EDGE_LOOP('',(#2788));
#600=EDGE_LOOP('',(#2789,#2790,#2791,#2792));
#601=EDGE_LOOP('',(#2793,#2794,#2795,#2796));
#602=EDGE_LOOP('',(#2797,#2798,#2799,#2800));
#603=EDGE_LOOP('',(#2801,#2802));
#604=EDGE_LOOP('',(#2803));
#605=EDGE_LOOP('',(#2804,#2805,#2806,#2807));
#606=EDGE_LOOP('',(#2808));
#607=EDGE_LOOP('',(#2809));
#608=EDGE_LOOP('',(#2810,#2811,#2812,#2813,#2814));
#609=EDGE_LOOP('',(#2815,#2816,#2817,#2818));
#610=EDGE_LOOP('',(#2819,#2820,#2821,#2822));
#611=EDGE_LOOP('',(#2823,#2824,#2825,#2826));
#612=EDGE_LOOP('',(#2827,#2828,#2829,#2830));
#613=EDGE_LOOP('',(#2831,#2832,#2833,#2834,#2835,#2836,#2837));
#614=EDGE_LOOP('',(#2838,#2839,#2840,#2841));
#615=EDGE_LOOP('',(#2842,#2843,#2844,#2845));
#616=EDGE_LOOP('',(#2846,#2847,#2848,#2849));
#617=EDGE_LOOP('',(#2850,#2851,#2852,#2853));
#618=EDGE_LOOP('',(#2854,#2855,#2856,#2857,#2858));
#619=EDGE_LOOP('',(#2859,#2860,#2861,#2862,#2863,#2864,#2865));
#620=EDGE_LOOP('',(#2866,#2867,#2868,#2869));
#621=EDGE_LOOP('',(#2870,#2871,#2872,#2873,#2874,#2875));
#622=EDGE_LOOP('',(#2876,#2877,#2878,#2879,#2880,#2881));
#623=EDGE_LOOP('',(#2882,#2883,#2884,#2885));
#624=EDGE_LOOP('',(#2886,#2887,#2888,#2889));
#625=EDGE_LOOP('',(#2890,#2891,#2892,#2893));
#626=EDGE_LOOP('',(#2894,#2895,#2896,#2897,#2898,#2899,#2900,#2901,#2902));
#627=EDGE_LOOP('',(#2903,#2904,#2905,#2906,#2907));
#628=EDGE_LOOP('',(#2908,#2909,#2910,#2911,#2912));
#629=EDGE_LOOP('',(#2913,#2914,#2915,#2916,#2917));
#630=EDGE_LOOP('',(#2918,#2919,#2920,#2921,#2922,#2923));
#631=EDGE_LOOP('',(#2924));
#632=EDGE_LOOP('',(#2925));
#633=EDGE_LOOP('',(#2926,#2927,#2928,#2929,#2930,#2931));
#634=EDGE_LOOP('',(#2932,#2933,#2934,#2935,#2936,#2937));
#635=EDGE_LOOP('',(#2938,#2939,#2940,#2941,#2942,#2943));
#636=EDGE_LOOP('',(#2944,#2945,#2946,#2947,#2948,#2949));
#637=EDGE_LOOP('',(#2950,#2951,#2952,#2953,#2954,#2955));
#638=EDGE_LOOP('',(#2956,#2957,#2958,#2959,#2960,#2961));
#639=EDGE_LOOP('',(#2962,#2963,#2964,#2965,#2966,#2967));
#640=EDGE_LOOP('',(#2968,#2969,#2970,#2971,#2972,#2973));
#641=EDGE_LOOP('',(#2974,#2975,#2976,#2977,#2978));
#642=EDGE_LOOP('',(#2979));
#643=EDGE_LOOP('',(#2980));
#644=EDGE_LOOP('',(#2981,#2982,#2983,#2984,#2985));
#645=EDGE_LOOP('',(#2986,#2987,#2988,#2989,#2990,#2991));
#646=EDGE_LOOP('',(#2992,#2993,#2994,#2995,#2996));
#647=EDGE_LOOP('',(#2997,#2998,#2999,#3000));
#648=EDGE_LOOP('',(#3001,#3002,#3003,#3004));
#649=EDGE_LOOP('',(#3005,#3006,#3007,#3008));
#650=EDGE_LOOP('',(#3009,#3010,#3011,#3012));
#651=EDGE_LOOP('',(#3013,#3014,#3015,#3016));
#652=EDGE_LOOP('',(#3017,#3018,#3019,#3020));
#653=EDGE_LOOP('',(#3021,#3022,#3023,#3024));
#654=EDGE_LOOP('',(#3025,#3026,#3027,#3028));
#655=EDGE_LOOP('',(#3029,#3030,#3031,#3032));
#656=EDGE_LOOP('',(#3033,#3034,#3035,#3036));
#657=EDGE_LOOP('',(#3037,#3038,#3039,#3040));
#658=EDGE_LOOP('',(#3041,#3042,#3043,#3044));
#659=EDGE_LOOP('',(#3045,#3046,#3047,#3048));
#660=EDGE_LOOP('',(#3049,#3050,#3051,#3052));
#661=EDGE_LOOP('',(#3053,#3054,#3055,#3056));
#662=EDGE_LOOP('',(#3057,#3058,#3059,#3060));
#663=EDGE_LOOP('',(#3061,#3062,#3063,#3064));
#664=EDGE_LOOP('',(#3065,#3066,#3067,#3068));
#665=EDGE_LOOP('',(#3069,#3070,#3071,#3072));
#666=EDGE_LOOP('',(#3073,#3074,#3075,#3076));
#667=EDGE_LOOP('',(#3077,#3078,#3079,#3080));
#668=EDGE_LOOP('',(#3081,#3082,#3083,#3084));
#669=EDGE_LOOP('',(#3085,#3086,#3087,#3088));
#670=EDGE_LOOP('',(#3089,#3090,#3091,#3092));
#671=EDGE_LOOP('',(#3093,#3094,#3095,#3096));
#672=EDGE_LOOP('',(#3097,#3098,#3099,#3100));
#673=EDGE_LOOP('',(#3101,#3102,#3103,#3104));
#674=EDGE_LOOP('',(#3105,#3106,#3107,#3108));
#675=EDGE_LOOP('',(#3109,#3110,#3111,#3112));
#676=EDGE_LOOP('',(#3113,#3114,#3115,#3116));
#677=EDGE_LOOP('',(#3117,#3118,#3119,#3120));
#678=EDGE_LOOP('',(#3121,#3122,#3123,#3124));
#679=EDGE_LOOP('',(#3125,#3126,#3127,#3128));
#680=EDGE_LOOP('',(#3129,#3130,#3131,#3132));
#681=EDGE_LOOP('',(#3133,#3134,#3135,#3136));
#682=EDGE_LOOP('',(#3137,#3138,#3139,#3140,#3141));
#683=EDGE_LOOP('',(#3142,#3143,#3144,#3145));
#684=EDGE_LOOP('',(#3146,#3147,#3148,#3149,#3150,#3151,#3152,#3153,#3154,
#3155,#3156,#3157,#3158,#3159,#3160,#3161,#3162,#3163,#3164,#3165,#3166,
#3167,#3168,#3169,#3170,#3171,#3172,#3173,#3174,#3175,#3176,#3177,#3178,
#3179,#3180,#3181,#3182,#3183,#3184));
#685=EDGE_LOOP('',(#3185,#3186,#3187,#3188,#3189));
#686=EDGE_LOOP('',(#3190,#3191,#3192,#3193,#3194,#3195,#3196,#3197,#3198,
#3199,#3200,#3201,#3202,#3203,#3204,#3205,#3206,#3207,#3208,#3209,#3210,
#3211,#3212,#3213,#3214,#3215,#3216,#3217,#3218,#3219,#3220,#3221,#3222,
#3223,#3224,#3225,#3226,#3227,#3228));
#687=EDGE_LOOP('',(#3229,#3230,#3231,#3232,#3233));
#688=EDGE_LOOP('',(#3234,#3235,#3236,#3237));
#689=EDGE_LOOP('',(#3238,#3239,#3240,#3241,#3242,#3243));
#690=EDGE_LOOP('',(#3244,#3245,#3246,#3247));
#691=EDGE_LOOP('',(#3248,#3249,#3250,#3251));
#692=EDGE_LOOP('',(#3252,#3253,#3254,#3255));
#693=EDGE_LOOP('',(#3256,#3257,#3258,#3259));
#694=EDGE_LOOP('',(#3260,#3261,#3262,#3263));
#695=EDGE_LOOP('',(#3264,#3265,#3266,#3267));
#696=EDGE_LOOP('',(#3268,#3269,#3270,#3271));
#697=EDGE_LOOP('',(#3272,#3273,#3274,#3275));
#698=EDGE_LOOP('',(#3276,#3277,#3278,#3279));
#699=EDGE_LOOP('',(#3280,#3281,#3282,#3283));
#700=EDGE_LOOP('',(#3284));
#701=EDGE_LOOP('',(#3285));
#702=EDGE_LOOP('',(#3286,#3287,#3288,#3289));
#703=EDGE_LOOP('',(#3290));
#704=EDGE_LOOP('',(#3291));
#705=EDGE_LOOP('',(#3292,#3293,#3294,#3295));
#706=EDGE_LOOP('',(#3296,#3297,#3298,#3299));
#707=EDGE_LOOP('',(#3300,#3301,#3302,#3303));
#708=EDGE_LOOP('',(#3304));
#709=EDGE_LOOP('',(#3305));
#710=EDGE_LOOP('',(#3306,#3307,#3308,#3309));
#711=EDGE_LOOP('',(#3310));
#712=EDGE_LOOP('',(#3311));
#713=EDGE_LOOP('',(#3312,#3313,#3314,#3315));
#714=EDGE_LOOP('',(#3316));
#715=EDGE_LOOP('',(#3317,#3318,#3319,#3320));
#716=EDGE_LOOP('',(#3321,#3322,#3323,#3324));
#717=EDGE_LOOP('',(#3325,#3326,#3327,#3328));
#718=EDGE_LOOP('',(#3329));
#719=EDGE_LOOP('',(#3330));
#720=EDGE_LOOP('',(#3331,#3332,#3333,#3334));
#721=EDGE_LOOP('',(#3335,#3336,#3337));
#722=EDGE_LOOP('',(#3338,#3339,#3340));
#723=EDGE_LOOP('',(#3341,#3342,#3343,#3344));
#724=EDGE_LOOP('',(#3345,#3346,#3347,#3348));
#725=EDGE_LOOP('',(#3349,#3350,#3351,#3352));
#726=EDGE_LOOP('',(#3353,#3354,#3355,#3356));
#727=EDGE_LOOP('',(#3357,#3358,#3359));
#728=EDGE_LOOP('',(#3360,#3361,#3362));
#729=EDGE_LOOP('',(#3363,#3364,#3365,#3366));
#730=EDGE_LOOP('',(#3367,#3368,#3369,#3370,#3371));
#731=EDGE_LOOP('',(#3372,#3373,#3374,#3375,#3376,#3377,#3378,#3379));
#732=EDGE_LOOP('',(#3380,#3381,#3382,#3383,#3384));
#733=EDGE_LOOP('',(#3385,#3386,#3387,#3388,#3389));
#734=EDGE_LOOP('',(#3390,#3391,#3392,#3393,#3394));
#735=EDGE_LOOP('',(#3395,#3396,#3397,#3398,#3399));
#736=EDGE_LOOP('',(#3400,#3401,#3402,#3403,#3404));
#737=EDGE_LOOP('',(#3405));
#738=EDGE_LOOP('',(#3406,#3407,#3408,#3409));
#739=EDGE_LOOP('',(#3410,#3411,#3412,#3413,#3414));
#740=EDGE_LOOP('',(#3415,#3416,#3417,#3418));
#741=EDGE_LOOP('',(#3419,#3420,#3421,#3422));
#742=EDGE_LOOP('',(#3423,#3424,#3425));
#743=EDGE_LOOP('',(#3426,#3427,#3428,#3429));
#744=EDGE_LOOP('',(#3430,#3431,#3432,#3433));
#745=EDGE_LOOP('',(#3434,#3435,#3436,#3437));
#746=EDGE_LOOP('',(#3438,#3439,#3440,#3441));
#747=EDGE_LOOP('',(#3442,#3443,#3444,#3445));
#748=EDGE_LOOP('',(#3446,#3447,#3448));
#749=EDGE_LOOP('',(#3449,#3450,#3451,#3452));
#750=EDGE_LOOP('',(#3453,#3454,#3455,#3456));
#751=EDGE_LOOP('',(#3457,#3458,#3459,#3460,#3461));
#752=EDGE_LOOP('',(#3462));
#753=EDGE_LOOP('',(#3463,#3464,#3465,#3466));
#754=EDGE_LOOP('',(#3467,#3468,#3469,#3470,#3471,#3472));
#755=EDGE_LOOP('',(#3473,#3474,#3475));
#756=EDGE_LOOP('',(#3476,#3477,#3478,#3479));
#757=EDGE_LOOP('',(#3480,#3481,#3482,#3483));
#758=EDGE_LOOP('',(#3484,#3485,#3486));
#759=EDGE_LOOP('',(#3487,#3488,#3489,#3490));
#760=EDGE_LOOP('',(#3491,#3492,#3493,#3494));
#761=EDGE_LOOP('',(#3495,#3496,#3497,#3498));
#762=EDGE_LOOP('',(#3499,#3500,#3501,#3502));
#763=EDGE_LOOP('',(#3503,#3504,#3505,#3506));
#764=EDGE_LOOP('',(#3507,#3508,#3509));
#765=EDGE_LOOP('',(#3510,#3511,#3512));
#766=EDGE_LOOP('',(#3513,#3514,#3515,#3516,#3517));
#767=EDGE_LOOP('',(#3518,#3519,#3520,#3521,#3522,#3523,#3524,#3525,#3526));
#768=EDGE_LOOP('',(#3527,#3528,#3529,#3530,#3531));
#769=EDGE_LOOP('',(#3532,#3533,#3534,#3535,#3536));
#770=EDGE_LOOP('',(#3537,#3538,#3539,#3540,#3541,#3542,#3543));
#771=EDGE_LOOP('',(#3544,#3545,#3546,#3547,#3548,#3549,#3550,#3551,#3552,
#3553,#3554,#3555));
#772=EDGE_LOOP('',(#3556,#3557,#3558,#3559,#3560,#3561,#3562));
#773=EDGE_LOOP('',(#3563));
#774=EDGE_LOOP('',(#3564));
#775=EDGE_LOOP('',(#3565,#3566,#3567,#3568));
#776=EDGE_LOOP('',(#3569,#3570,#3571,#3572,#3573));
#777=EDGE_LOOP('',(#3574,#3575,#3576,#3577,#3578,#3579));
#778=EDGE_LOOP('',(#3580));
#779=EDGE_LOOP('',(#3581));
#780=EDGE_LOOP('',(#3582,#3583,#3584,#3585,#3586));
#781=EDGE_LOOP('',(#3587));
#782=EDGE_LOOP('',(#3588));
#783=EDGE_LOOP('',(#3589,#3590,#3591,#3592));
#784=EDGE_LOOP('',(#3593,#3594,#3595,#3596));
#785=EDGE_LOOP('',(#3597,#3598,#3599));
#786=EDGE_LOOP('',(#3600,#3601,#3602));
#787=EDGE_LOOP('',(#3603,#3604,#3605));
#788=EDGE_LOOP('',(#3606,#3607,#3608));
#789=EDGE_LOOP('',(#3609,#3610,#3611,#3612,#3613,#3614,#3615,#3616,#3617,
#3618,#3619,#3620,#3621,#3622));
#790=EDGE_LOOP('',(#3623,#3624,#3625,#3626));
#791=EDGE_LOOP('',(#3627,#3628,#3629,#3630,#3631,#3632));
#792=EDGE_LOOP('',(#3633,#3634,#3635,#3636,#3637));
#793=EDGE_LOOP('',(#3638,#3639,#3640,#3641,#3642,#3643));
#794=EDGE_LOOP('',(#3644,#3645,#3646,#3647,#3648));
#795=EDGE_LOOP('',(#3649,#3650,#3651,#3652,#3653,#3654,#3655,#3656,#3657));
#796=EDGE_LOOP('',(#3658,#3659,#3660,#3661,#3662,#3663,#3664,#3665,#3666));
#797=EDGE_LOOP('',(#3667,#3668,#3669,#3670));
#798=EDGE_LOOP('',(#3671,#3672,#3673,#3674,#3675));
#799=EDGE_LOOP('',(#3676,#3677,#3678));
#800=EDGE_LOOP('',(#3679,#3680,#3681));
#801=EDGE_LOOP('',(#3682,#3683,#3684,#3685,#3686));
#802=EDGE_LOOP('',(#3687,#3688,#3689,#3690));
#803=EDGE_LOOP('',(#3691,#3692,#3693));
#804=EDGE_LOOP('',(#3694,#3695,#3696));
#805=EDGE_LOOP('',(#3697,#3698,#3699,#3700,#3701,#3702,#3703,#3704,#3705,
#3706,#3707,#3708,#3709,#3710));
#806=EDGE_LOOP('',(#3711,#3712,#3713,#3714));
#807=EDGE_LOOP('',(#3715,#3716,#3717,#3718));
#808=EDGE_LOOP('',(#3719,#3720,#3721,#3722));
#809=EDGE_LOOP('',(#3723,#3724,#3725,#3726,#3727));
#810=EDGE_LOOP('',(#3728));
#811=EDGE_LOOP('',(#3729));
#812=EDGE_LOOP('',(#3730,#3731,#3732,#3733,#3734));
#813=EDGE_LOOP('',(#3735,#3736,#3737,#3738,#3739,#3740,#3741,#3742,#3743));
#814=EDGE_LOOP('',(#3744,#3745,#3746,#3747,#3748,#3749,#3750,#3751,#3752,
#3753,#3754,#3755));
#815=EDGE_LOOP('',(#3756,#3757,#3758));
#816=EDGE_LOOP('',(#3759,#3760,#3761));
#817=EDGE_LOOP('',(#3762,#3763,#3764,#3765,#3766));
#818=EDGE_LOOP('',(#3767,#3768,#3769,#3770));
#819=EDGE_LOOP('',(#3771,#3772,#3773,#3774,#3775,#3776));
#820=EDGE_LOOP('',(#3777,#3778,#3779,#3780));
#821=EDGE_LOOP('',(#3781,#3782,#3783,#3784));
#822=EDGE_LOOP('',(#3785,#3786,#3787,#3788,#3789));
#823=EDGE_LOOP('',(#3790,#3791,#3792,#3793,#3794,#3795));
#824=EDGE_LOOP('',(#3796));
#825=EDGE_LOOP('',(#3797));
#826=EDGE_LOOP('',(#3798,#3799,#3800,#3801,#3802,#3803));
#827=EDGE_LOOP('',(#3804,#3805,#3806,#3807,#3808,#3809));
#828=EDGE_LOOP('',(#3810,#3811,#3812,#3813,#3814));
#829=EDGE_LOOP('',(#3815));
#830=EDGE_LOOP('',(#3816));
#831=EDGE_LOOP('',(#3817,#3818,#3819,#3820,#3821));
#832=EDGE_LOOP('',(#3822,#3823,#3824,#3825,#3826,#3827));
#833=EDGE_LOOP('',(#3828,#3829,#3830,#3831,#3832));
#834=EDGE_LOOP('',(#3833,#3834,#3835,#3836));
#835=EDGE_LOOP('',(#3837));
#836=EDGE_LOOP('',(#3838));
#837=EDGE_LOOP('',(#3839,#3840,#3841,#3842));
#838=EDGE_LOOP('',(#3843,#3844,#3845,#3846));
#839=EDGE_LOOP('',(#3847,#3848,#3849,#3850));
#840=EDGE_LOOP('',(#3851));
#841=EDGE_LOOP('',(#3852));
#842=EDGE_LOOP('',(#3853,#3854,#3855,#3856));
#843=EDGE_LOOP('',(#3857,#3858,#3859,#3860));
#844=EDGE_LOOP('',(#3861,#3862,#3863,#3864));
#845=EDGE_LOOP('',(#3865));
#846=EDGE_LOOP('',(#3866));
#847=EDGE_LOOP('',(#3867,#3868,#3869,#3870));
#848=EDGE_LOOP('',(#3871));
#849=EDGE_LOOP('',(#3872));
#850=EDGE_LOOP('',(#3873,#3874,#3875,#3876));
#851=EDGE_LOOP('',(#3877,#3878,#3879,#3880));
#852=EDGE_LOOP('',(#3881,#3882,#3883,#3884,#3885,#3886,#3887,#3888));
#853=EDGE_LOOP('',(#3889));
#854=EDGE_LOOP('',(#3890));
#855=EDGE_LOOP('',(#3891,#3892,#3893,#3894));
#856=EDGE_LOOP('',(#3895,#3896,#3897,#3898));
#857=EDGE_LOOP('',(#3899,#3900,#3901,#3902));
#858=EDGE_LOOP('',(#3903,#3904,#3905,#3906,#3907,#3908,#3909,#3910));
#859=EDGE_LOOP('',(#3911));
#860=EDGE_LOOP('',(#3912));
#861=EDGE_LOOP('',(#3913,#3914,#3915,#3916));
#862=EDGE_LOOP('',(#3917,#3918,#3919,#3920));
#863=EDGE_LOOP('',(#3921,#3922,#3923,#3924));
#864=EDGE_LOOP('',(#3925,#3926,#3927,#3928));
#865=EDGE_LOOP('',(#3929,#3930,#3931,#3932));
#866=EDGE_LOOP('',(#3933,#3934,#3935));
#867=EDGE_LOOP('',(#3936,#3937,#3938));
#868=EDGE_LOOP('',(#3939,#3940,#3941));
#869=EDGE_LOOP('',(#3942,#3943,#3944));
#870=EDGE_LOOP('',(#3945,#3946,#3947,#3948));
#871=EDGE_LOOP('',(#3949,#3950,#3951));
#872=EDGE_LOOP('',(#3952,#3953,#3954));
#873=EDGE_LOOP('',(#3955,#3956,#3957,#3958));
#874=EDGE_LOOP('',(#3959,#3960,#3961));
#875=EDGE_LOOP('',(#3962,#3963,#3964,#3965));
#876=EDGE_LOOP('',(#3966,#3967,#3968,#3969));
#877=EDGE_LOOP('',(#3970,#3971,#3972));
#878=EDGE_LOOP('',(#3973,#3974,#3975,#3976));
#879=EDGE_LOOP('',(#3977,#3978,#3979,#3980));
#880=EDGE_LOOP('',(#3981,#3982,#3983,#3984));
#881=EDGE_LOOP('',(#3985,#3986,#3987,#3988));
#882=EDGE_LOOP('',(#3989,#3990,#3991,#3992));
#883=EDGE_LOOP('',(#3993,#3994,#3995,#3996));
#884=EDGE_LOOP('',(#3997,#3998,#3999,#4000));
#885=EDGE_LOOP('',(#4001,#4002,#4003,#4004));
#886=EDGE_LOOP('',(#4005,#4006,#4007,#4008));
#887=EDGE_LOOP('',(#4009,#4010,#4011,#4012));
#888=EDGE_LOOP('',(#4013,#4014,#4015,#4016));
#889=EDGE_LOOP('',(#4017,#4018,#4019,#4020));
#890=EDGE_LOOP('',(#4021,#4022,#4023,#4024));
#891=EDGE_LOOP('',(#4025,#4026,#4027,#4028));
#892=CIRCLE('',#4508,11.05);
#893=CIRCLE('',#4509,11.05);
#894=CIRCLE('',#4510,0.499999999999999);
#895=CIRCLE('',#4512,0.5);
#896=CIRCLE('',#4513,11.5);
#897=CIRCLE('',#4515,0.500000000000007);
#898=CIRCLE('',#4516,0.499999999999999);
#899=CIRCLE('',#4518,57.5);
#900=CIRCLE('',#4519,57.5);
#901=CIRCLE('',#4520,0.499999999999989);
#902=CIRCLE('',#4522,59.7);
#903=CIRCLE('',#4524,0.5);
#904=CIRCLE('',#4525,0.5);
#905=CIRCLE('',#4526,0.5);
#906=CIRCLE('',#4528,0.5);
#907=CIRCLE('',#4529,0.5);
#908=CIRCLE('',#4533,0.5);
#909=CIRCLE('',#4534,0.5);
#910=CIRCLE('',#4536,0.5);
#911=CIRCLE('',#4537,0.5);
#912=CIRCLE('',#4539,0.5);
#913=CIRCLE('',#4542,60.);
#914=CIRCLE('',#4543,60.5);
#915=CIRCLE('',#4545,58.);
#916=CIRCLE('',#4548,57.5);
#917=CIRCLE('',#4550,58.1);
#918=CIRCLE('',#4552,59.9);
#919=CIRCLE('',#4554,60.5);
#920=CIRCLE('',#4555,60.5);
#921=CIRCLE('',#4556,60.5);
#922=CIRCLE('',#4557,60.5);
#923=CIRCLE('',#4560,0.8);
#924=CIRCLE('',#4563,15.9482352626124);
#925=CIRCLE('',#4564,0.5);
#926=CIRCLE('',#4565,16.0506668396737);
#927=CIRCLE('',#4566,16.0506668396737);
#928=CIRCLE('',#4568,58.8542048431045);
#929=CIRCLE('',#4569,58.8542048431045);
#930=CIRCLE('',#4571,11.);
#931=CIRCLE('',#4573,0.5);
#932=CIRCLE('',#4574,59.1053266566364);
#933=CIRCLE('',#4575,59.1053266566364);
#934=CIRCLE('',#4577,59.3535533905933);
#935=CIRCLE('',#4578,59.3535533905933);
#936=CIRCLE('',#4580,0.5);
#937=CIRCLE('',#4581,59.5);
#938=CIRCLE('',#4582,59.5);
#939=CIRCLE('',#4584,59.5);
#940=CIRCLE('',#4585,59.5);
#941=CIRCLE('',#4587,0.5);
#942=CIRCLE('',#4588,59.3535533905933);
#943=CIRCLE('',#4589,59.3535533905933);
#944=CIRCLE('',#4591,59.111396327342);
#945=CIRCLE('',#4592,59.111396327342);
#946=CIRCLE('',#4594,0.5);
#947=CIRCLE('',#4595,58.8448662431924);
#948=CIRCLE('',#4596,58.8448662431924);
#949=CIRCLE('',#4598,16.0431770496114);
#950=CIRCLE('',#4599,16.0431770496114);
#951=CIRCLE('',#4601,0.5);
#952=CIRCLE('',#4602,15.9561537431677);
#953=CIRCLE('',#4604,11.);
#954=CIRCLE('',#4606,0.5);
#955=CIRCLE('',#4607,10.5);
#956=CIRCLE('',#4608,10.5);
#957=CIRCLE('',#4610,10.5);
#958=CIRCLE('',#4611,10.5);
#959=CIRCLE('',#4613,0.5);
#960=CIRCLE('',#4616,3.4544);
#961=CIRCLE('',#4633,3.4544);
#962=CIRCLE('',#4635,3.96875);
#963=CIRCLE('',#4653,3.96875);
#964=CIRCLE('',#4655,3.4544);
#965=CIRCLE('',#4656,3.4544);
#966=CIRCLE('',#4659,3.4544);
#967=CIRCLE('',#4660,3.4544);
#968=CIRCLE('',#4664,4.05000000000002);
#969=CIRCLE('',#4667,7.94);
#970=CIRCLE('',#4670,7.94);
#971=CIRCLE('',#4674,7.94);
#972=CIRCLE('',#4677,7.94);
#973=CIRCLE('',#4680,7.94);
#974=CIRCLE('',#4681,7.6);
#975=CIRCLE('',#4683,7.6);
#976=CIRCLE('',#4685,7.94);
#977=CIRCLE('',#4687,7.94);
#978=CIRCLE('',#4689,7.6);
#979=CIRCLE('',#4691,7.6);
#980=CIRCLE('',#4693,7.94);
#981=CIRCLE('',#4695,7.94);
#982=CIRCLE('',#4697,7.44);
#983=CIRCLE('',#4700,7.94);
#984=CIRCLE('',#4702,7.14);
#985=CIRCLE('',#4706,0.5);
#986=CIRCLE('',#4707,56.1500768331935);
#987=CIRCLE('',#4708,0.499999999998982);
#988=CIRCLE('',#4709,56.5341874729922);
#989=CIRCLE('',#4711,0.5);
#990=CIRCLE('',#4713,0.5);
#991=CIRCLE('',#4714,0.50000000000007);
#992=CIRCLE('',#4716,0.5);
#993=CIRCLE('',#4718,0.499999999999984);
#994=CIRCLE('',#4719,0.499999999999998);
#995=CIRCLE('',#4721,0.499999999999986);
#996=CIRCLE('',#4722,0.499999999999986);
#997=CIRCLE('',#4724,0.5);
#998=CIRCLE('',#4726,0.500000000000001);
#999=CIRCLE('',#4728,20.);
#1000=CIRCLE('',#4730,12.);
#1001=CIRCLE('',#4731,12.);
#1002=CIRCLE('',#4732,0.5);
#1003=CIRCLE('',#4733,11.5);
#1004=CIRCLE('',#4735,8.45);
#1005=CIRCLE('',#4737,12.);
#1006=CIRCLE('',#4742,0.5);
#1007=CIRCLE('',#4744,0.5);
#1008=CIRCLE('',#4745,0.5);
#1009=CIRCLE('',#4747,7.95);
#1010=CIRCLE('',#4748,0.5);
#1011=CIRCLE('',#4750,0.5);
#1012=CIRCLE('',#4757,0.5);
#1013=CIRCLE('',#4758,0.5);
#1014=CIRCLE('',#4761,8.45);
#1015=CIRCLE('',#4762,0.5);
#1016=CIRCLE('',#4763,7.95);
#1017=CIRCLE('',#4765,19.9567770454363);
#1018=CIRCLE('',#4766,0.5);
#1019=CIRCLE('',#4767,20.0425817450355);
#1020=CIRCLE('',#4768,20.0425817450355);
#1021=CIRCLE('',#4771,51.);
#1022=CIRCLE('',#4772,51.);
#1023=CIRCLE('',#4774,0.5);
#1024=CIRCLE('',#4775,0.5);
#1025=CIRCLE('',#4778,0.5);
#1026=CIRCLE('',#4780,0.5);
#1027=CIRCLE('',#4784,0.499999999999991);
#1028=CIRCLE('',#4785,0.499999999999993);
#1029=CIRCLE('',#4787,0.5);
#1030=CIRCLE('',#4789,0.50000000000002);
#1031=CIRCLE('',#4791,0.5);
#1032=CIRCLE('',#4798,12.6);
#1033=CIRCLE('',#4799,12.6);
#1034=CIRCLE('',#4800,12.3);
#1035=CIRCLE('',#4802,12.6);
#1036=CIRCLE('',#4803,12.6);
#1037=CIRCLE('',#4805,10.6);
#1038=CIRCLE('',#4807,12.3);
#1039=CIRCLE('',#4809,11.);
#1040=CIRCLE('',#4811,10.5);
#1041=CIRCLE('',#4812,10.5);
#1042=CIRCLE('',#4814,10.5);
#1043=CIRCLE('',#4815,10.5);
#1044=CIRCLE('',#4822,10.8828427124746);
#1045=CIRCLE('',#4823,10.8828427124746);
#1046=CIRCLE('',#4824,0.4);
#1047=CIRCLE('',#4825,11.);
#1048=CIRCLE('',#4826,11.);
#1049=CIRCLE('',#4829,10.6171572875254);
#1050=CIRCLE('',#4830,10.6171572875254);
#1051=CIRCLE('',#4832,0.4);
#1052=CIRCLE('',#4833,11.);
#1053=CIRCLE('',#4834,11.);
#1054=CIRCLE('',#4836,11.);
#1055=CIRCLE('',#4837,11.);
#1056=CIRCLE('',#4839,10.8828427124746);
#1057=CIRCLE('',#4841,10.6171572875254);
#1058=CIRCLE('',#4842,0.4);
#1059=CIRCLE('',#4843,0.4);
#1060=CIRCLE('',#4845,0.400000000000002);
#1061=CIRCLE('',#4846,10.3343145750508);
#1062=CIRCLE('',#4847,0.4);
#1063=CIRCLE('',#4849,0.400000000000003);
#1064=CIRCLE('',#4851,0.400000000000003);
#1065=CIRCLE('',#4854,0.4);
#1066=CIRCLE('',#4856,8.35);
#1067=CIRCLE('',#4858,0.4);
#1068=CIRCLE('',#4860,10.3343145750508);
#1069=CIRCLE('',#4861,0.4);
#1070=CIRCLE('',#4863,8.35);
#1071=CIRCLE('',#4865,7.95);
#1072=CIRCLE('',#4866,7.95);
#1073=CIRCLE('',#4867,0.4);
#1074=CIRCLE('',#4869,7.95);
#1075=CIRCLE('',#4870,7.95);
#1076=CIRCLE('',#4871,7.95);
#1077=CIRCLE('',#4874,0.4);
#1078=CIRCLE('',#4875,0.4);
#1079=CIRCLE('',#4877,0.400000000000001);
#1080=CIRCLE('',#4878,0.4);
#1081=CIRCLE('',#4882,8.35);
#1082=CIRCLE('',#4887,15.2928932188134);
#1083=CIRCLE('',#4888,0.5);
#1084=CIRCLE('',#4889,15.6464466094067);
#1085=CIRCLE('',#4890,15.6464466094067);
#1086=CIRCLE('',#4892,15.8535533905933);
#1087=CIRCLE('',#4893,15.8535533905933);
#1088=CIRCLE('',#4895,11.);
#1089=CIRCLE('',#4897,0.5);
#1090=CIRCLE('',#4898,16.);
#1091=CIRCLE('',#4899,16.);
#1092=CIRCLE('',#4901,16.);
#1093=CIRCLE('',#4902,16.);
#1094=CIRCLE('',#4904,0.5);
#1095=CIRCLE('',#4905,15.5);
#1096=CIRCLE('',#4907,11.);
#1097=CIRCLE('',#4909,0.5);
#1098=CIRCLE('',#4910,10.5);
#1099=CIRCLE('',#4911,10.5);
#1100=CIRCLE('',#4913,10.5);
#1101=CIRCLE('',#4914,10.5);
#1102=CIRCLE('',#4916,0.5);
#1103=CIRCLE('',#4919,10.5);
#1104=CIRCLE('',#4920,10.5);
#1105=CIRCLE('',#4922,8.265);
#1106=CIRCLE('',#4924,7.965);
#1107=CIRCLE('',#4926,7.965);
#1108=CIRCLE('',#4928,8.265);
#1109=CIRCLE('',#4932,11.);
#1110=CIRCLE('',#4933,10.8);
#1111=CIRCLE('',#4935,11.);
#1112=CIRCLE('',#4937,10.8);
#1113=CIRCLE('',#4939,8.);
#1114=CIRCLE('',#4941,8.);
#1115=CIRCLE('',#4945,0.85);
#1116=CIRCLE('',#4946,0.85);
#1117=CIRCLE('',#4948,0.85);
#1118=CIRCLE('',#4949,0.85);
#1119=CIRCLE('',#4951,9.9);
#1120=CIRCLE('',#4952,7.6);
#1121=CIRCLE('',#4957,7.6);
#1122=CIRCLE('',#4958,9.9);
#1123=LINE('',#6285,#1353);
#1124=LINE('',#7363,#1354);
#1125=LINE('',#7367,#1355);
#1126=LINE('',#7424,#1356);
#1127=LINE('',#7425,#1357);
#1128=LINE('',#7480,#1358);
#1129=LINE('',#7481,#1359);
#1130=LINE('',#7484,#1360);
#1131=LINE('',#7506,#1361);
#1132=LINE('',#7509,#1362);
#1133=LINE('',#7552,#1363);
#1134=LINE('',#7553,#1364);
#1135=LINE('',#7609,#1365);
#1136=LINE('',#7611,#1366);
#1137=LINE('',#7619,#1367);
#1138=LINE('',#7636,#1368);
#1139=LINE('',#7655,#1369);
#1140=LINE('',#7670,#1370);
#1141=LINE('',#7682,#1371);
#1142=LINE('',#7694,#1372);
#1143=LINE('',#7706,#1373);
#1144=LINE('',#7728,#1374);
#1145=LINE('',#7735,#1375);
#1146=LINE('',#7777,#1376);
#1147=LINE('',#7825,#1377);
#1148=LINE('',#7876,#1378);
#1149=LINE('',#7927,#1379);
#1150=LINE('',#7975,#1380);
#1151=LINE('',#8026,#1381);
#1152=LINE('',#8074,#1382);
#1153=LINE('',#8125,#1383);
#1154=LINE('',#8176,#1384);
#1155=LINE('',#8224,#1385);
#1156=LINE('',#8275,#1386);
#1157=LINE('',#8326,#1387);
#1158=LINE('',#8374,#1388);
#1159=LINE('',#8425,#1389);
#1160=LINE('',#8473,#1390);
#1161=LINE('',#8524,#1391);
#1162=LINE('',#8566,#1392);
#1163=LINE('',#8583,#1393);
#1164=LINE('',#8608,#1394);
#1165=LINE('',#8633,#1395);
#1166=LINE('',#8657,#1396);
#1167=LINE('',#8682,#1397);
#1168=LINE('',#8707,#1398);
#1169=LINE('',#8731,#1399);
#1170=LINE('',#8755,#1400);
#1171=LINE('',#8781,#1401);
#1172=LINE('',#8805,#1402);
#1173=LINE('',#8829,#1403);
#1174=LINE('',#8855,#1404);
#1175=LINE('',#8879,#1405);
#1176=LINE('',#8903,#1406);
#1177=LINE('',#8928,#1407);
#1178=LINE('',#8953,#1408);
#1179=LINE('',#8977,#1409);
#1180=LINE('',#10319,#1410);
#1181=LINE('',#10323,#1411);
#1182=LINE('',#10328,#1412);
#1183=LINE('',#10330,#1413);
#1184=LINE('',#10332,#1414);
#1185=LINE('',#10333,#1415);
#1186=LINE('',#10338,#1416);
#1187=LINE('',#10339,#1417);
#1188=LINE('',#10342,#1418);
#1189=LINE('',#10344,#1419);
#1190=LINE('',#10345,#1420);
#1191=LINE('',#10348,#1421);
#1192=LINE('',#10353,#1422);
#1193=LINE('',#10355,#1423);
#1194=LINE('',#10357,#1424);
#1195=LINE('',#10358,#1425);
#1196=LINE('',#10363,#1426);
#1197=LINE('',#10364,#1427);
#1198=LINE('',#10367,#1428);
#1199=LINE('',#10369,#1429);
#1200=LINE('',#10370,#1430);
#1201=LINE('',#10373,#1431);
#1202=LINE('',#10383,#1432);
#1203=LINE('',#10389,#1433);
#1204=LINE('',#10397,#1434);
#1205=LINE('',#10403,#1435);
#1206=LINE('',#10409,#1436);
#1207=LINE('',#10413,#1437);
#1208=LINE('',#10417,#1438);
#1209=LINE('',#10478,#1439);
#1210=LINE('',#10481,#1440);
#1211=LINE('',#10484,#1441);
#1212=LINE('',#11012,#1442);
#1213=LINE('',#11138,#1443);
#1214=LINE('',#11150,#1444);
#1215=LINE('',#11154,#1445);
#1216=LINE('',#11155,#1446);
#1217=LINE('',#11159,#1447);
#1218=LINE('',#11164,#1448);
#1219=LINE('',#11168,#1449);
#1220=LINE('',#11180,#1450);
#1221=LINE('',#11183,#1451);
#1222=LINE('',#11186,#1452);
#1223=LINE('',#11187,#1453);
#1224=LINE('',#11190,#1454);
#1225=LINE('',#11191,#1455);
#1226=LINE('',#11196,#1456);
#1227=LINE('',#11203,#1457);
#1228=LINE('',#11219,#1458);
#1229=LINE('',#11222,#1459);
#1230=LINE('',#11231,#1460);
#1231=LINE('',#11235,#1461);
#1232=LINE('',#11236,#1462);
#1233=LINE('',#11240,#1463);
#1234=LINE('',#11375,#1464);
#1235=LINE('',#11720,#1465);
#1236=LINE('',#11795,#1466);
#1237=LINE('',#11802,#1467);
#1238=LINE('',#11809,#1468);
#1239=LINE('',#11816,#1469);
#1240=LINE('',#11820,#1470);
#1241=LINE('',#11825,#1471);
#1242=LINE('',#11829,#1472);
#1243=LINE('',#11833,#1473);
#1244=LINE('',#11834,#1474);
#1245=LINE('',#11837,#1475);
#1246=LINE('',#11838,#1476);
#1247=LINE('',#11841,#1477);
#1248=LINE('',#11842,#1478);
#1249=LINE('',#11845,#1479);
#1250=LINE('',#11846,#1480);
#1251=LINE('',#11849,#1481);
#1252=LINE('',#11851,#1482);
#1253=LINE('',#11858,#1483);
#1254=LINE('',#11860,#1484);
#1255=LINE('',#11901,#1485);
#1256=LINE('',#11946,#1486);
#1257=LINE('',#12141,#1487);
#1258=LINE('',#12146,#1488);
#1259=LINE('',#12156,#1489);
#1260=LINE('',#12159,#1490);
#1261=LINE('',#12436,#1491);
#1262=LINE('',#12438,#1492);
#1263=LINE('',#12440,#1493);
#1264=LINE('',#12447,#1494);
#1265=LINE('',#12448,#1495);
#1266=LINE('',#12451,#1496);
#1267=LINE('',#12455,#1497);
#1268=LINE('',#12474,#1498);
#1269=LINE('',#12478,#1499);
#1270=LINE('',#12482,#1500);
#1271=LINE('',#12485,#1501);
#1272=LINE('',#12529,#1502);
#1273=LINE('',#12544,#1503);
#1274=LINE('',#12566,#1504);
#1275=LINE('',#12574,#1505);
#1276=LINE('',#12581,#1506);
#1277=LINE('',#12585,#1507);
#1278=LINE('',#12589,#1508);
#1279=LINE('',#12597,#1509);
#1280=LINE('',#12602,#1510);
#1281=LINE('',#12606,#1511);
#1282=LINE('',#12612,#1512);
#1283=LINE('',#12620,#1513);
#1284=LINE('',#12626,#1514);
#1285=LINE('',#12631,#1515);
#1286=LINE('',#12633,#1516);
#1287=LINE('',#12635,#1517);
#1288=LINE('',#12639,#1518);
#1289=LINE('',#12641,#1519);
#1290=LINE('',#12643,#1520);
#1291=LINE('',#12647,#1521);
#1292=LINE('',#12649,#1522);
#1293=LINE('',#12650,#1523);
#1294=LINE('',#12653,#1524);
#1295=LINE('',#12654,#1525);
#1296=LINE('',#12657,#1526);
#1297=LINE('',#12658,#1527);
#1298=LINE('',#12662,#1528);
#1299=LINE('',#12667,#1529);
#1300=LINE('',#12668,#1530);
#1301=LINE('',#12670,#1531);
#1302=LINE('',#12672,#1532);
#1303=LINE('',#12674,#1533);
#1304=LINE('',#12675,#1534);
#1305=LINE('',#12682,#1535);
#1306=LINE('',#12684,#1536);
#1307=LINE('',#12685,#1537);
#1308=LINE('',#12689,#1538);
#1309=LINE('',#12691,#1539);
#1310=LINE('',#12692,#1540);
#1311=LINE('',#12696,#1541);
#1312=LINE('',#12698,#1542);
#1313=LINE('',#12699,#1543);
#1314=LINE('',#12703,#1544);
#1315=LINE('',#12705,#1545);
#1316=LINE('',#12706,#1546);
#1317=LINE('',#12708,#1547);
#1318=LINE('',#12709,#1548);
#1319=LINE('',#12713,#1549);
#1320=LINE('',#12715,#1550);
#1321=LINE('',#12716,#1551);
#1322=LINE('',#12720,#1552);
#1323=LINE('',#12722,#1553);
#1324=LINE('',#12723,#1554);
#1325=LINE('',#12725,#1555);
#1326=LINE('',#12726,#1556);
#1327=LINE('',#12730,#1557);
#1328=LINE('',#12732,#1558);
#1329=LINE('',#12733,#1559);
#1330=LINE('',#12735,#1560);
#1331=LINE('',#12736,#1561);
#1332=LINE('',#12738,#1562);
#1333=LINE('',#12739,#1563);
#1334=LINE('',#12743,#1564);
#1335=LINE('',#12745,#1565);
#1336=LINE('',#12746,#1566);
#1337=LINE('',#12748,#1567);
#1338=LINE('',#12749,#1568);
#1339=LINE('',#12751,#1569);
#1340=LINE('',#12752,#1570);
#1341=LINE('',#12754,#1571);
#1342=LINE('',#12755,#1572);
#1343=LINE('',#12757,#1573);
#1344=LINE('',#12758,#1574);
#1345=LINE('',#12760,#1575);
#1346=LINE('',#12761,#1576);
#1347=LINE('',#12763,#1577);
#1348=LINE('',#12764,#1578);
#1349=LINE('',#12766,#1579);
#1350=LINE('',#12767,#1580);
#1351=LINE('',#12769,#1581);
#1352=LINE('',#12770,#1582);
#1353=VECTOR('',#5010,11.05);
#1354=VECTOR('',#5045,10.);
#1355=VECTOR('',#5048,10.);
#1356=VECTOR('',#5055,10.);
#1357=VECTOR('',#5056,10.);
#1358=VECTOR('',#5061,10.);
#1359=VECTOR('',#5062,10.);
#1360=VECTOR('',#5065,10.);
#1361=VECTOR('',#5068,10.);
#1362=VECTOR('',#5071,10.);
#1363=VECTOR('',#5078,10.);
#1364=VECTOR('',#5079,10.);
#1365=VECTOR('',#5084,10.);
#1366=VECTOR('',#5085,10.);
#1367=VECTOR('',#5090,10.);
#1368=VECTOR('',#5119,60.5);
#1369=VECTOR('',#5146,37.5);
#1370=VECTOR('',#5165,59.25);
#1371=VECTOR('',#5180,59.5);
#1372=VECTOR('',#5195,59.25);
#1373=VECTOR('',#5210,37.5);
#1374=VECTOR('',#5239,10.5);
#1375=VECTOR('',#5248,3.55);
#1376=VECTOR('',#5253,3.55);
#1377=VECTOR('',#5256,3.55);
#1378=VECTOR('',#5259,3.55);
#1379=VECTOR('',#5262,3.55);
#1380=VECTOR('',#5265,3.55);
#1381=VECTOR('',#5268,3.55);
#1382=VECTOR('',#5271,3.55);
#1383=VECTOR('',#5274,3.55);
#1384=VECTOR('',#5277,3.55);
#1385=VECTOR('',#5280,3.55);
#1386=VECTOR('',#5283,3.55);
#1387=VECTOR('',#5286,3.55);
#1388=VECTOR('',#5289,3.55);
#1389=VECTOR('',#5292,3.55);
#1390=VECTOR('',#5295,3.55);
#1391=VECTOR('',#5298,3.55);
#1392=VECTOR('',#5303,3.96875);
#1393=VECTOR('',#5308,3.96875);
#1394=VECTOR('',#5311,3.96875);
#1395=VECTOR('',#5314,3.96875);
#1396=VECTOR('',#5317,3.96875);
#1397=VECTOR('',#5320,3.96875);
#1398=VECTOR('',#5323,3.96875);
#1399=VECTOR('',#5326,3.96875);
#1400=VECTOR('',#5329,3.96875);
#1401=VECTOR('',#5332,3.96875);
#1402=VECTOR('',#5335,3.96875);
#1403=VECTOR('',#5338,3.96875);
#1404=VECTOR('',#5341,3.96875);
#1405=VECTOR('',#5344,3.96875);
#1406=VECTOR('',#5347,3.96875);
#1407=VECTOR('',#5350,3.96875);
#1408=VECTOR('',#5353,3.96875);
#1409=VECTOR('',#5356,3.96875);
#1410=VECTOR('',#5375,1.775);
#1411=VECTOR('',#5380,3.85);
#1412=VECTOR('',#5385,10.);
#1413=VECTOR('',#5386,10.);
#1414=VECTOR('',#5387,10.);
#1415=VECTOR('',#5388,10.);
#1416=VECTOR('',#5393,10.);
#1417=VECTOR('',#5394,10.);
#1418=VECTOR('',#5397,10.);
#1419=VECTOR('',#5398,10.);
#1420=VECTOR('',#5399,10.);
#1421=VECTOR('',#5404,10.);
#1422=VECTOR('',#5409,10.);
#1423=VECTOR('',#5410,10.);
#1424=VECTOR('',#5411,10.);
#1425=VECTOR('',#5412,10.);
#1426=VECTOR('',#5417,10.);
#1427=VECTOR('',#5418,10.);
#1428=VECTOR('',#5421,10.);
#1429=VECTOR('',#5422,10.);
#1430=VECTOR('',#5423,10.);
#1431=VECTOR('',#5428,10.);
#1432=VECTOR('',#5441,7.6);
#1433=VECTOR('',#5448,7.94);
#1434=VECTOR('',#5459,7.6);
#1435=VECTOR('',#5466,7.94);
#1436=VECTOR('',#5475,7.69);
#1437=VECTOR('',#5480,7.94);
#1438=VECTOR('',#5485,7.54);
#1439=VECTOR('',#5512,10.);
#1440=VECTOR('',#5515,10.);
#1441=VECTOR('',#5518,10.);
#1442=VECTOR('',#5535,10.);
#1443=VECTOR('',#5542,35.);
#1444=VECTOR('',#5555,10.);
#1445=VECTOR('',#5558,10.);
#1446=VECTOR('',#5559,10.);
#1447=VECTOR('',#5564,12.);
#1448=VECTOR('',#5569,10.);
#1449=VECTOR('',#5574,10.);
#1450=VECTOR('',#5591,10.);
#1451=VECTOR('',#5594,10.);
#1452=VECTOR('',#5597,10.);
#1453=VECTOR('',#5598,10.);
#1454=VECTOR('',#5601,10.);
#1455=VECTOR('',#5602,10.);
#1456=VECTOR('',#5607,10.);
#1457=VECTOR('',#5618,10.);
#1458=VECTOR('',#5639,10.);
#1459=VECTOR('',#5642,35.5);
#1460=VECTOR('',#5655,10.);
#1461=VECTOR('',#5660,10.);
#1462=VECTOR('',#5661,10.);
#1463=VECTOR('',#5668,10.);
#1464=VECTOR('',#5679,10.);
#1465=VECTOR('',#5692,10.);
#1466=VECTOR('',#5707,12.45);
#1467=VECTOR('',#5716,12.6);
#1468=VECTOR('',#5725,12.45);
#1469=VECTOR('',#5732,10.);
#1470=VECTOR('',#5735,10.);
#1471=VECTOR('',#5740,10.);
#1472=VECTOR('',#5743,10.);
#1473=VECTOR('',#5748,10.);
#1474=VECTOR('',#5749,10.);
#1475=VECTOR('',#5752,10.);
#1476=VECTOR('',#5753,10.);
#1477=VECTOR('',#5756,10.);
#1478=VECTOR('',#5757,10.);
#1479=VECTOR('',#5760,10.);
#1480=VECTOR('',#5761,10.);
#1481=VECTOR('',#5764,10.);
#1482=VECTOR('',#5765,10.);
#1483=VECTOR('',#5766,10.);
#1484=VECTOR('',#5767,10.);
#1485=VECTOR('',#5768,10.);
#1486=VECTOR('',#5769,10.);
#1487=VECTOR('',#5784,11.);
#1488=VECTOR('',#5789,10.75);
#1489=VECTOR('',#5802,11.);
#1490=VECTOR('',#5805,10.);
#1491=VECTOR('',#5838,10.);
#1492=VECTOR('',#5839,10.);
#1493=VECTOR('',#5840,10.);
#1494=VECTOR('',#5841,10.);
#1495=VECTOR('',#5842,10.);
#1496=VECTOR('',#5845,10.);
#1497=VECTOR('',#5850,10.);
#1498=VECTOR('',#5877,7.95);
#1499=VECTOR('',#5880,10.);
#1500=VECTOR('',#5883,10.);
#1501=VECTOR('',#5888,10.);
#1502=VECTOR('',#5927,15.75);
#1503=VECTOR('',#5946,16.);
#1504=VECTOR('',#5975,10.5);
#1505=VECTOR('',#5986,10.5);
#1506=VECTOR('',#5995,8.115);
#1507=VECTOR('',#6000,7.965);
#1508=VECTOR('',#6005,8.115);
#1509=VECTOR('',#6016,10.9);
#1510=VECTOR('',#6023,11.);
#1511=VECTOR('',#6028,10.9);
#1512=VECTOR('',#6035,8.);
#1513=VECTOR('',#6046,0.85);
#1514=VECTOR('',#6053,0.85);
#1515=VECTOR('',#6058,10.);
#1516=VECTOR('',#6059,10.);
#1517=VECTOR('',#6060,10.);
#1518=VECTOR('',#6063,10.);
#1519=VECTOR('',#6064,10.);
#1520=VECTOR('',#6065,10.);
#1521=VECTOR('',#6070,10.);
#1522=VECTOR('',#6071,10.);
#1523=VECTOR('',#6072,10.);
#1524=VECTOR('',#6075,10.);
#1525=VECTOR('',#6076,10.);
#1526=VECTOR('',#6079,10.);
#1527=VECTOR('',#6080,10.);
#1528=VECTOR('',#6083,10.);
#1529=VECTOR('',#6088,10.);
#1530=VECTOR('',#6089,10.);
#1531=VECTOR('',#6092,10.);
#1532=VECTOR('',#6095,10.);
#1533=VECTOR('',#6098,10.);
#1534=VECTOR('',#6099,10.);
#1535=VECTOR('',#6108,10.);
#1536=VECTOR('',#6109,10.);
#1537=VECTOR('',#6110,10.);
#1538=VECTOR('',#6113,10.);
#1539=VECTOR('',#6114,10.);
#1540=VECTOR('',#6115,10.);
#1541=VECTOR('',#6118,10.);
#1542=VECTOR('',#6119,10.);
#1543=VECTOR('',#6120,10.);
#1544=VECTOR('',#6123,10.);
#1545=VECTOR('',#6124,10.);
#1546=VECTOR('',#6125,10.);
#1547=VECTOR('',#6128,10.);
#1548=VECTOR('',#6129,10.);
#1549=VECTOR('',#6132,10.);
#1550=VECTOR('',#6133,10.);
#1551=VECTOR('',#6134,10.);
#1552=VECTOR('',#6137,10.);
#1553=VECTOR('',#6138,10.);
#1554=VECTOR('',#6139,10.);
#1555=VECTOR('',#6142,10.);
#1556=VECTOR('',#6143,10.);
#1557=VECTOR('',#6146,10.);
#1558=VECTOR('',#6147,10.);
#1559=VECTOR('',#6148,10.);
#1560=VECTOR('',#6151,10.);
#1561=VECTOR('',#6152,10.);
#1562=VECTOR('',#6155,10.);
#1563=VECTOR('',#6156,10.);
#1564=VECTOR('',#6159,10.);
#1565=VECTOR('',#6160,10.);
#1566=VECTOR('',#6161,10.);
#1567=VECTOR('',#6164,10.);
#1568=VECTOR('',#6165,10.);
#1569=VECTOR('',#6168,10.);
#1570=VECTOR('',#6169,10.);
#1571=VECTOR('',#6172,10.);
#1572=VECTOR('',#6173,10.);
#1573=VECTOR('',#6176,10.);
#1574=VECTOR('',#6177,10.);
#1575=VECTOR('',#6180,10.);
#1576=VECTOR('',#6181,10.);
#1577=VECTOR('',#6184,10.);
#1578=VECTOR('',#6185,10.);
#1579=VECTOR('',#6188,10.);
#1580=VECTOR('',#6189,10.);
#1581=VECTOR('',#6192,10.);
#1582=VECTOR('',#6193,10.);
#1583=B_SPLINE_CURVE_WITH_KNOTS('',3,(#6237,#6238,#6239,#6240,#6241,#6242,
#6243,#6244,#6245,#6246,#6247,#6248,#6249,#6250,#6251,#6252,#6253,#6254,
#6255,#6256,#6257,#6258,#6259,#6260,#6261),.UNSPECIFIED.,.F.,.F.,(4,3,3,
3,3,3,3,3,4),(-6.96374017603088,-6.4663927644122,-5.96904535279352,-5.47169794117485,
-4.97435052955617,-4.31122064739794,-3.97965570631882,-3.6480907652397,
-3.48231742770748),.UNSPECIFIED.);
#1584=B_SPLINE_CURVE_WITH_KNOTS('',3,(#6262,#6263,#6264,#6265,#6266,#6267,
#6268,#6269,#6270,#6271,#6272,#6273,#6274,#6275,#6276,#6277,#6278,#6279,
#6280,#6281,#6282,#6283),.UNSPECIFIED.,.F.,.F.,(4,3,3,3,3,3,3,4),(-3.48231742770748,
-2.98483567920087,-2.65318727040077,-1.98989045280058,-1.65824204400048,
-0.994945226400289,-0.497472613200144,0.),.UNSPECIFIED.);
#1585=B_SPLINE_CURVE_WITH_KNOTS('',3,(#6359,#6360,#6361,#6362,#6363,#6364,
#6365,#6366,#6367,#6368,#6369,#6370,#6371,#6372,#6373,#6374,#6375),
 .UNSPECIFIED.,.T.,.F.,(4,1,1,1,1,1,1,1,1,1,1,1,1,1,4),(-7.85398163397448,
-7.40518268346166,-6.95638373294883,-6.35798513226506,-6.05878583192317,
-5.4603872312394,-5.16118793089752,-4.56278933021375,-4.26359002987186,
-3.96439072952998,-3.36599212884621,-2.91719317833338,-2.46839422782055,
-2.01959527730772,-1.5707963267949),.UNSPECIFIED.);
#1586=B_SPLINE_CURVE_WITH_KNOTS('',3,(#6677,#6678,#6679,#6680,#6681,#6682,
#6683,#6684,#6685,#6686,#6687,#6688,#6689,#6690,#6691,#6692,#6693,#6694,
#6695),.UNSPECIFIED.,.T.,.F.,(4,1,1,1,1,1,1,1,1,1,1,1,1,1,1,1,4),(1.5707963267949,
2.01959527730772,2.46839422782055,2.91719317833338,3.36599212884621,3.66519142918809,
3.96439072952998,4.26359002987186,4.56278933021375,5.16118793089752,5.4603872312394,
5.75958653158129,6.05878583192317,6.35798513226506,6.95638373294883,7.40518268346166,
7.85398163397448),.UNSPECIFIED.);
#1587=B_SPLINE_CURVE_WITH_KNOTS('',3,(#6702,#6703,#6704,#6705,#6706,#6707,
#6708,#6709,#6710,#6711,#6712,#6713,#6714,#6715,#6716,#6717,#6718),
 .UNSPECIFIED.,.T.,.F.,(4,1,1,1,1,1,1,1,1,1,1,1,1,1,4),(-7.85398163397448,
-7.40518268346166,-6.95638373294883,-6.35798513226506,-6.05878583192317,
-5.4603872312394,-5.16118793089752,-4.56278933021375,-4.26359002987186,
-3.66519142918809,-3.36599212884621,-2.91719317833338,-2.46839422782055,
-2.01959527730772,-1.5707963267949),.UNSPECIFIED.);
#1588=B_SPLINE_CURVE_WITH_KNOTS('',3,(#6789,#6790,#6791,#6792,#6793,#6794,
#6795,#6796,#6797,#6798,#6799,#6800,#6801,#6802,#6803,#6804,#6805),
 .UNSPECIFIED.,.T.,.F.,(4,1,1,1,1,1,1,1,1,1,1,1,1,1,4),(1.5707963267949,
2.01959527730772,2.46839422782055,2.91719317833338,3.36599212884621,3.66519142918809,
4.26359002987186,4.56278933021375,5.16118793089752,5.4603872312394,6.05878583192317,
6.35798513226506,6.95638373294883,7.40518268346166,7.85398163397448),
 .UNSPECIFIED.);
#1589=B_SPLINE_CURVE_WITH_KNOTS('',3,(#7107,#7108,#7109,#7110,#7111,#7112,
#7113,#7114,#7115,#7116,#7117,#7118,#7119,#7120,#7121,#7122,#7123,#7124,
#7125),.UNSPECIFIED.,.T.,.F.,(4,1,1,1,1,1,1,1,1,1,1,1,1,1,1,1,4),(-7.85398163397448,
-7.40518268346166,-6.95638373294883,-6.35798513226506,-6.05878583192317,
-5.75958653158129,-5.4603872312394,-5.16118793089752,-4.56278933021375,
-4.26359002987186,-3.96439072952998,-3.66519142918809,-3.36599212884621,
-2.91719317833338,-2.46839422782055,-2.01959527730772,-1.5707963267949),
 .UNSPECIFIED.);
#1590=B_SPLINE_CURVE_WITH_KNOTS('',3,(#7204,#7205,#7206,#7207,#7208,#7209,
#7210,#7211,#7212,#7213,#7214,#7215,#7216,#7217,#7218,#7219,#7220,#7221,
#7222),.UNSPECIFIED.,.T.,.F.,(4,1,1,1,1,1,1,1,1,1,1,1,1,1,1,1,4),(1.5707963267949,
2.01959527730772,2.46839422782055,2.91719317833338,3.36599212884621,3.66519142918809,
3.96439072952998,4.26359002987186,4.56278933021375,5.16118793089752,5.4603872312394,
5.75958653158129,6.05878583192317,6.35798513226506,6.95638373294883,7.40518268346166,
7.85398163397448),.UNSPECIFIED.);
#1591=B_SPLINE_CURVE_WITH_KNOTS('',3,(#7306,#7307,#7308,#7309,#7310,#7311,
#7312,#7313,#7314,#7315,#7316,#7317,#7318,#7319,#7320,#7321,#7322,#7323,
#7324,#7325,#7326,#7327,#7328,#7329,#7330,#7331,#7332,#7333,#7334,#7335,
#7336,#7337,#7338,#7339,#7340,#7341,#7342,#7343,#7344,#7345,#7346,#7347,
#7348,#7349,#7350,#7351,#7352,#7353,#7354),.UNSPECIFIED.,.T.,.F.,(4,3,3,
3,3,3,3,3,3,3,3,3,3,3,3,3,4),(-7.85398163397448,-7.40518268346166,-6.95638373294883,
-6.35798513226506,-6.05878583192317,-5.75958653158129,-5.4603872312394,
-5.16118793089752,-4.56278933021375,-4.26359002987186,-3.96439072952998,
-3.66519142918809,-3.36599212884621,-2.91719317833338,-2.46839422782055,
-2.01959527730772,-1.5707963267949),.UNSPECIFIED.);
#1592=B_SPLINE_CURVE_WITH_KNOTS('',3,(#7368,#7369,#7370,#7371,#7372,#7373,
#7374,#7375,#7376,#7377,#7378,#7379,#7380,#7381),.UNSPECIFIED.,.F.,.F.,
(4,2,2,2,2,2,4),(-0.107735848698753,-0.106444261823602,-0.0883469717566643,
-0.066319510943676,-0.0374807627664021,0.,0.000337595117382213),
 .UNSPECIFIED.);
#1593=B_SPLINE_CURVE_WITH_KNOTS('',3,(#7410,#7411,#7412,#7413,#7414),
 .UNSPECIFIED.,.F.,.F.,(4,1,4),(-0.0157172487336364,-0.00785862436681818,
0.),.UNSPECIFIED.);
#1594=B_SPLINE_CURVE_WITH_KNOTS('',3,(#7415,#7416,#7417,#7418,#7419),
 .UNSPECIFIED.,.F.,.F.,(4,1,4),(0.,0.00785862436681818,0.0157172487336364),
 .UNSPECIFIED.);
#1595=B_SPLINE_CURVE_WITH_KNOTS('',3,(#7454,#7455,#7456,#7457,#7458),
 .UNSPECIFIED.,.F.,.F.,(4,1,4),(-0.0157178998040451,-0.00785894990202256,
0.),.UNSPECIFIED.);
#1596=B_SPLINE_CURVE_WITH_KNOTS('',3,(#7459,#7460,#7461,#7462,#7463),
 .UNSPECIFIED.,.F.,.F.,(4,1,4),(0.,0.00785894990202256,0.0157178998040451),
 .UNSPECIFIED.);
#1597=B_SPLINE_CURVE_WITH_KNOTS('',3,(#7466,#7467,#7468,#7469,#7470,#7471,
#7472,#7473,#7474,#7475,#7476,#7477,#7478,#7479),.UNSPECIFIED.,.F.,.F.,
(4,2,2,2,2,2,4),(-0.223861268001062,-0.223443477302026,-0.194339722291654,
-0.164729520611538,-0.141542392329575,-0.123303095351833,-0.110634522469103),
 .UNSPECIFIED.);
#1598=B_SPLINE_CURVE_WITH_KNOTS('',3,(#7485,#7486,#7487,#7488),
 .UNSPECIFIED.,.F.,.F.,(4,4),(0.0740823244647065,0.0764086756743631),
 .UNSPECIFIED.);
#1599=B_SPLINE_CURVE_WITH_KNOTS('',3,(#7491,#7492,#7493,#7494,#7495,#7496,
#7497,#7498,#7499,#7500,#7501,#7502,#7503,#7504),.UNSPECIFIED.,.F.,.F.,
(4,2,2,2,2,2,4),(-0.0929971191805655,-0.0825534377905717,-0.0675173790191802,
-0.0484024414197425,-0.0239924691911123,0.,0.000344417085089716),
 .UNSPECIFIED.);
#1600=B_SPLINE_CURVE_WITH_KNOTS('',3,(#7538,#7539,#7540,#7541,#7542),
 .UNSPECIFIED.,.F.,.F.,(4,1,4),(-0.0157179005447003,-0.00785895027235015,
-1.02053899928999E-18),.UNSPECIFIED.);
#1601=B_SPLINE_CURVE_WITH_KNOTS('',3,(#7543,#7544,#7545,#7546,#7547),
 .UNSPECIFIED.,.F.,.F.,(4,1,4),(1.02053899928999E-18,0.00785895027235015,
0.0157179005447003),.UNSPECIFIED.);
#1602=B_SPLINE_CURVE_WITH_KNOTS('',3,(#7582,#7583,#7584,#7585,#7586),
 .UNSPECIFIED.,.F.,.F.,(4,1,4),(-0.0157172480339581,-0.00785862401697905,
0.),.UNSPECIFIED.);
#1603=B_SPLINE_CURVE_WITH_KNOTS('',3,(#7587,#7588,#7589,#7590,#7591),
 .UNSPECIFIED.,.F.,.F.,(4,1,4),(0.,0.00785862401697905,0.0157172480339581),
 .UNSPECIFIED.);
#1604=B_SPLINE_CURVE_WITH_KNOTS('',3,(#7595,#7596,#7597,#7598,#7599,#7600,
#7601,#7602,#7603,#7604,#7605,#7606,#7607,#7608),.UNSPECIFIED.,.F.,.F.,
(4,2,2,2,2,2,4),(-0.184461049750143,-0.184182901618329,-0.153302110980918,
-0.129541566131588,-0.1113929118506,-0.0964823661623737,-0.0954182142898604),
 .UNSPECIFIED.);
#1605=B_SPLINE_CURVE_WITH_KNOTS('',3,(#7615,#7616,#7617,#7618),
 .UNSPECIFIED.,.F.,.F.,(4,4),(0.21992163243666,0.222247983646316),
 .UNSPECIFIED.);
#1606=B_SPLINE_CURVE_WITH_KNOTS('',3,(#7737,#7738,#7739,#7740,#7741,#7742,
#7743,#7744,#7745,#7746,#7747,#7748,#7749),.UNSPECIFIED.,.F.,.F.,(4,3,3,
3,4),(107.889370485171,108.385448006876,109.379809915196,110.374171823516,
111.368533731836),.UNSPECIFIED.);
#1607=B_SPLINE_CURVE_WITH_KNOTS('',3,(#7752,#7753,#7754,#7755,#7756,#7757,
#7758,#7759,#7760,#7761,#7762,#7763,#7764,#7765,#7766,#7767,#7768,#7769,
#7770,#7771,#7772,#7773),.UNSPECIFIED.,.F.,.F.,(4,3,3,3,3,3,3,4),(-109.6055207498,
-109.379809915196,-108.385448006876,-107.391086098556,-106.396724190236,
-105.402362281916,-104.408000373596,-104.360350287381),.UNSPECIFIED.);
#1608=B_SPLINE_CURVE_WITH_KNOTS('',3,(#7778,#7779,#7780,#7781,#7782,#7783,
#7784,#7785,#7786,#7787,#7788,#7789,#7790,#7791,#7792,#7793,#7794,#7795,
#7796,#7797,#7798,#7799),.UNSPECIFIED.,.F.,.F.,(4,3,3,3,3,3,3,4),(101.606185177992,
102.419276556956,103.413638465276,104.408000373596,105.402362281916,106.396724190236,
107.391086098556,107.889370485171),.UNSPECIFIED.);
#1609=B_SPLINE_CURVE_WITH_KNOTS('',3,(#7800,#7801,#7802,#7803,#7804,#7805,
#7806,#7807,#7808,#7809,#7810,#7811,#7812,#7813,#7814,#7815,#7816,#7817,
#7818,#7819,#7820,#7821),.UNSPECIFIED.,.F.,.F.,(4,3,3,3,3,3,3,4),(-104.360350287381,
-103.413638465276,-102.419276556956,-101.424914648636,-100.430552740316,
-99.4361908319964,-98.4418289236764,-98.0771649802013),.UNSPECIFIED.);
#1610=B_SPLINE_CURVE_WITH_KNOTS('',3,(#7826,#7827,#7828,#7829,#7830,#7831,
#7832,#7833,#7834,#7835,#7836,#7837,#7838,#7839,#7840,#7841,#7842,#7843,
#7844,#7845,#7846,#7847,#7848,#7849,#7850),.UNSPECIFIED.,.F.,.F.,(4,3,3,
3,3,3,3,3,4),(95.3229998708118,95.4587431987165,96.4531051070365,97.4474670153564,
98.4418289236764,99.4361908319964,100.430552740316,101.424914648636,101.606185177992),
 .UNSPECIFIED.);
#1611=B_SPLINE_CURVE_WITH_KNOTS('',3,(#7851,#7852,#7853,#7854,#7855,#7856,
#7857,#7858,#7859,#7860,#7861,#7862,#7863,#7864,#7865,#7866,#7867,#7868,
#7869,#7870,#7871,#7872),.UNSPECIFIED.,.F.,.F.,(4,3,3,3,3,3,3,4),(-98.0771649802013,
-97.4474670153564,-96.4531051070365,-95.4587431987165,-94.4643812903965,
-93.4700193820766,-92.4756574737566,-91.7939796730218),.UNSPECIFIED.);
#1612=B_SPLINE_CURVE_WITH_KNOTS('',3,(#7877,#7878,#7879,#7880,#7881,#7882,
#7883,#7884,#7885,#7886,#7887,#7888,#7889,#7890,#7891,#7892,#7893,#7894,
#7895,#7896,#7897,#7898),.UNSPECIFIED.,.F.,.F.,(4,3,3,3,3,3,3,4),(89.0398145636323,
89.4925717487967,90.4869336571167,91.4812955654367,92.4756574737566,93.4700193820766,
94.4643812903965,95.3229998708118),.UNSPECIFIED.);
#1613=B_SPLINE_CURVE_WITH_KNOTS('',3,(#7899,#7900,#7901,#7902,#7903,#7904,
#7905,#7906,#7907,#7908,#7909,#7910,#7911,#7912,#7913,#7914,#7915,#7916,
#7917,#7918,#7919,#7920,#7921,#7922,#7923),.UNSPECIFIED.,.F.,.F.,(4,3,3,
3,3,3,3,3,4),(-91.7939796730218,-91.4812955654366,-90.4869336571167,-89.4925717487967,
-88.4982098404768,-87.5038479321568,-86.5094860238368,-85.5151241155169,
-85.5107943658422),.UNSPECIFIED.);
#1614=B_SPLINE_CURVE_WITH_KNOTS('',3,(#7928,#7929,#7930,#7931,#7932,#7933,
#7934,#7935,#7936,#7937,#7938,#7939,#7940,#7941,#7942,#7943,#7944,#7945,
#7946,#7947,#7948,#7949),.UNSPECIFIED.,.F.,.F.,(4,3,3,3,3,3,3,4),(82.7566292564527,
83.526400298877,84.5207622071969,85.5151241155169,86.5094860238368,87.5038479321568,
88.4982098404767,89.0398145636323),.UNSPECIFIED.);
#1615=B_SPLINE_CURVE_WITH_KNOTS('',3,(#7950,#7951,#7952,#7953,#7954,#7955,
#7956,#7957,#7958,#7959,#7960,#7961,#7962,#7963,#7964,#7965,#7966,#7967,
#7968,#7969,#7970,#7971),.UNSPECIFIED.,.F.,.F.,(4,3,3,3,3,3,3,4),(-85.5107943658422,
-84.5207622071969,-83.526400298877,-82.532038390557,-81.537676482237,-80.5433145739171,
-79.5489526655971,-79.2276090586625),.UNSPECIFIED.);
#1616=B_SPLINE_CURVE_WITH_KNOTS('',3,(#7976,#7977,#7978,#7979,#7980,#7981,
#7982,#7983,#7984,#7985,#7986,#7987,#7988,#7989,#7990,#7991,#7992,#7993,
#7994,#7995,#7996,#7997,#7998,#7999,#8000),.UNSPECIFIED.,.F.,.F.,(4,3,3,
3,3,3,3,3,4),(76.473443949273,76.5658669406372,77.5602288489572,78.5545907572771,
79.5489526655971,80.543314573917,81.537676482237,82.532038390557,82.7566292564527),
 .UNSPECIFIED.);
#1617=B_SPLINE_CURVE_WITH_KNOTS('',3,(#8001,#8002,#8003,#8004,#8005,#8006,
#8007,#8008,#8009,#8010,#8011,#8012,#8013,#8014,#8015,#8016,#8017,#8018,
#8019,#8020,#8021,#8022),.UNSPECIFIED.,.F.,.F.,(4,3,3,3,3,3,3,4),(-79.2276090586625,
-78.5545907572771,-77.5602288489572,-76.5658669406372,-75.5715050323172,
-74.5771431239973,-73.5827812156773,-72.944423751483),.UNSPECIFIED.);
#1618=B_SPLINE_CURVE_WITH_KNOTS('',3,(#8027,#8028,#8029,#8030,#8031,#8032,
#8033,#8034,#8035,#8036,#8037,#8038,#8039,#8040,#8041,#8042,#8043,#8044,
#8045,#8046,#8047,#8048),.UNSPECIFIED.,.F.,.F.,(4,3,3,3,3,3,3,4),(70.1902586420935,
70.5996954907174,71.5940573990374,72.5884193073573,73.5827812156773,74.5771431239973,
75.5715050323172,76.473443949273),.UNSPECIFIED.);
#1619=B_SPLINE_CURVE_WITH_KNOTS('',3,(#8049,#8050,#8051,#8052,#8053,#8054,
#8055,#8056,#8057,#8058,#8059,#8060,#8061,#8062,#8063,#8064,#8065,#8066,
#8067,#8068,#8069,#8070),.UNSPECIFIED.,.F.,.F.,(4,3,3,3,3,3,3,4),(-72.944423751483,
-72.5884193073574,-71.5940573990374,-70.5996954907174,-69.6053335823975,
-68.6109716740775,-67.6166097657575,-66.6612384443034),.UNSPECIFIED.);
#1620=B_SPLINE_CURVE_WITH_KNOTS('',3,(#8075,#8076,#8077,#8078,#8079,#8080,
#8081,#8082,#8083,#8084,#8085,#8086,#8087,#8088,#8089,#8090,#8091,#8092,
#8093,#8094,#8095,#8096),.UNSPECIFIED.,.F.,.F.,(4,3,3,3,3,3,3,4),(63.9070733349139,
64.6335240407976,65.6278859491176,66.6222478574375,67.6166097657575,68.6109716740775,
69.6053335823974,70.1902586420935),.UNSPECIFIED.);
#1621=B_SPLINE_CURVE_WITH_KNOTS('',3,(#8097,#8098,#8099,#8100,#8101,#8102,
#8103,#8104,#8105,#8106,#8107,#8108,#8109,#8110,#8111,#8112,#8113,#8114,
#8115,#8116,#8117,#8118,#8119,#8120,#8121),.UNSPECIFIED.,.F.,.F.,(4,3,3,
3,3,3,3,3,4),(-66.6612384443034,-66.6222478574376,-65.6278859491176,-64.6335240407977,
-63.6391621324777,-62.6448002241577,-61.6504383158378,-60.6560764075178,
-60.3780531371238),.UNSPECIFIED.);
#1622=B_SPLINE_CURVE_WITH_KNOTS('',3,(#8126,#8127,#8128,#8129,#8130,#8131,
#8132,#8133,#8134,#8135,#8136,#8137,#8138,#8139,#8140,#8141,#8142,#8143,
#8144,#8145,#8146,#8147,#8148,#8149,#8150),.UNSPECIFIED.,.F.,.F.,(4,3,3,
3,3,3,3,3,4),(57.6238880277343,57.6729906825579,58.6673525908779,59.6617144991978,
60.6560764075178,61.6504383158377,62.6448002241577,63.6391621324777,63.9070733349139),
 .UNSPECIFIED.);
#1623=B_SPLINE_CURVE_WITH_KNOTS('',3,(#8151,#8152,#8153,#8154,#8155,#8156,
#8157,#8158,#8159,#8160,#8161,#8162,#8163,#8164,#8165,#8166,#8167,#8168,
#8169,#8170,#8171,#8172),.UNSPECIFIED.,.F.,.F.,(4,3,3,3,3,3,3,4),(-60.3780531371238,
-59.6617144991978,-58.6673525908779,-57.6729906825579,-56.6786287742379,
-55.684266865918,-54.689904957598,-54.0948678299441),.UNSPECIFIED.);
#1624=B_SPLINE_CURVE_WITH_KNOTS('',3,(#8177,#8178,#8179,#8180,#8181,#8182,
#8183,#8184,#8185,#8186,#8187,#8188,#8189,#8190,#8191,#8192,#8193,#8194,
#8195,#8196,#8197,#8198),.UNSPECIFIED.,.F.,.F.,(4,3,3,3,3,3,3,4),(51.3407027205547,
51.7068192326381,52.7011811409581,53.695543049278,54.689904957598,55.684266865918,
56.6786287742379,57.6238880277343),.UNSPECIFIED.);
#1625=B_SPLINE_CURVE_WITH_KNOTS('',3,(#8199,#8200,#8201,#8202,#8203,#8204,
#8205,#8206,#8207,#8208,#8209,#8210,#8211,#8212,#8213,#8214,#8215,#8216,
#8217,#8218,#8219,#8220),.UNSPECIFIED.,.F.,.F.,(4,3,3,3,3,3,3,4),(-54.0948678299441,
-53.695543049278,-52.7011811409581,-51.7068192326381,-50.7124573243181,
-49.7180954159982,-48.7237335076782,-47.8116825227646),.UNSPECIFIED.);
#1626=B_SPLINE_CURVE_WITH_KNOTS('',3,(#8225,#8226,#8227,#8228,#8229,#8230,
#8231,#8232,#8233,#8234,#8235,#8236,#8237,#8238,#8239,#8240,#8241,#8242,
#8243,#8244,#8245,#8246),.UNSPECIFIED.,.F.,.F.,(4,3,3,3,3,3,3,4),(45.0575174133751,
45.7406477827183,46.7350096910383,47.7293715993583,48.7237335076782,49.7180954159982,
50.7124573243181,51.3407027205547),.UNSPECIFIED.);
#1627=B_SPLINE_CURVE_WITH_KNOTS('',3,(#8247,#8248,#8249,#8250,#8251,#8252,
#8253,#8254,#8255,#8256,#8257,#8258,#8259,#8260,#8261,#8262,#8263,#8264,
#8265,#8266,#8267,#8268,#8269,#8270,#8271),.UNSPECIFIED.,.F.,.F.,(4,3,3,
3,3,3,3,3,4),(-47.8116825227646,-47.7293715993582,-46.7350096910383,-45.7406477827183,
-44.7462858743984,-43.7519239660784,-42.7575620577584,-41.7632001494385,
-41.528497215585),.UNSPECIFIED.);
#1628=B_SPLINE_CURVE_WITH_KNOTS('',3,(#8276,#8277,#8278,#8279,#8280,#8281,
#8282,#8283,#8284,#8285,#8286,#8287,#8288,#8289,#8290,#8291,#8292,#8293,
#8294,#8295,#8296,#8297,#8298,#8299,#8300),.UNSPECIFIED.,.F.,.F.,(4,3,3,
3,3,3,3,3,4),(38.7743321061955,38.7801144244786,39.7744763327985,40.7688382411185,
41.7632001494385,42.7575620577584,43.7519239660784,44.7462858743984,45.0575174133751),
 .UNSPECIFIED.);
#1629=B_SPLINE_CURVE_WITH_KNOTS('',3,(#8301,#8302,#8303,#8304,#8305,#8306,
#8307,#8308,#8309,#8310,#8311,#8312,#8313,#8314,#8315,#8316,#8317,#8318,
#8319,#8320,#8321,#8322),.UNSPECIFIED.,.F.,.F.,(4,3,3,3,3,3,3,4),(-41.528497215585,
-40.7688382411185,-39.7744763327985,-38.7801144244786,-37.7857525161586,
-36.7913906078387,-35.7970286995187,-35.2453119084054),.UNSPECIFIED.);
#1630=B_SPLINE_CURVE_WITH_KNOTS('',3,(#8327,#8328,#8329,#8330,#8331,#8332,
#8333,#8334,#8335,#8336,#8337,#8338,#8339,#8340,#8341,#8342,#8343,#8344,
#8345,#8346,#8347,#8348),.UNSPECIFIED.,.F.,.F.,(4,3,3,3,3,3,3,4),(32.491146799016,
32.8139429745588,33.8083048828788,34.8026667911987,35.7970286995187,36.7913906078386,
37.7857525161586,38.7743321061955),.UNSPECIFIED.);
#1631=B_SPLINE_CURVE_WITH_KNOTS('',3,(#8349,#8350,#8351,#8352,#8353,#8354,
#8355,#8356,#8357,#8358,#8359,#8360,#8361,#8362,#8363,#8364,#8365,#8366,
#8367,#8368,#8369,#8370),.UNSPECIFIED.,.F.,.F.,(4,3,3,3,3,3,3,4),(-35.2453119084054,
-34.8026667911987,-33.8083048828788,-32.8139429745588,-31.8195810662388,
-30.8252191579189,-29.8308572495989,-28.9621266012258),.UNSPECIFIED.);
#1632=B_SPLINE_CURVE_WITH_KNOTS('',3,(#8375,#8376,#8377,#8378,#8379,#8380,
#8381,#8382,#8383,#8384,#8385,#8386,#8387,#8388,#8389,#8390,#8391,#8392,
#8393,#8394,#8395,#8396),.UNSPECIFIED.,.F.,.F.,(4,3,3,3,3,3,3,4),(26.2079614918363,
26.847771524639,27.842133432959,28.8364953412789,29.8308572495989,30.8252191579189,
31.8195810662388,32.491146799016),.UNSPECIFIED.);
#1633=B_SPLINE_CURVE_WITH_KNOTS('',3,(#8397,#8398,#8399,#8400,#8401,#8402,
#8403,#8404,#8405,#8406,#8407,#8408,#8409,#8410,#8411,#8412,#8413,#8414,
#8415,#8416,#8417,#8418,#8419,#8420,#8421),.UNSPECIFIED.,.F.,.F.,(4,3,3,
3,3,3,3,3,4),(-28.9621266012258,-28.836495341279,-27.842133432959,-26.847771524639,
-25.8534096163191,-24.8590477079991,-23.8646857996791,-22.8703238913592,
-22.6789412940462),.UNSPECIFIED.);
#1634=B_SPLINE_CURVE_WITH_KNOTS('',3,(#8426,#8427,#8428,#8429,#8430,#8431,
#8432,#8433,#8434,#8435,#8436,#8437,#8438,#8439,#8440,#8441,#8442,#8443,
#8444,#8445,#8446,#8447),.UNSPECIFIED.,.F.,.F.,(4,3,3,3,3,3,3,4),(19.9247761846567,
20.8816000747192,21.8759619830392,22.8703238913592,23.8646857996791,24.8590477079991,
25.8534096163191,26.2079614918363),.UNSPECIFIED.);
#1635=B_SPLINE_CURVE_WITH_KNOTS('',3,(#8448,#8449,#8450,#8451,#8452,#8453,
#8454,#8455,#8456,#8457,#8458,#8459,#8460,#8461,#8462,#8463,#8464,#8465,
#8466,#8467,#8468,#8469),.UNSPECIFIED.,.F.,.F.,(4,3,3,3,3,3,3,4),(-22.6789412940462,
-21.8759619830392,-20.8816000747192,-19.8872381663993,-18.8928762580793,
-17.8985143497593,-16.9041524414394,-16.3957559868666),.UNSPECIFIED.);
#1636=B_SPLINE_CURVE_WITH_KNOTS('',3,(#8474,#8475,#8476,#8477,#8478,#8479,
#8480,#8481,#8482,#8483,#8484,#8485,#8486,#8487,#8488,#8489,#8490,#8491,
#8492,#8493,#8494,#8495,#8496,#8497,#8498),.UNSPECIFIED.,.F.,.F.,(4,3,3,
3,3,3,3,3,4),(13.6415908774772,13.9210667164795,14.9154286247995,15.9097905331194,
16.9041524414394,17.8985143497593,18.8928762580793,19.8872381663993,19.9247761846567),
 .UNSPECIFIED.);
#1637=B_SPLINE_CURVE_WITH_KNOTS('',3,(#8499,#8500,#8501,#8502,#8503,#8504,
#8505,#8506,#8507,#8508,#8509,#8510,#8511,#8512,#8513,#8514,#8515,#8516,
#8517,#8518,#8519,#8520),.UNSPECIFIED.,.F.,.F.,(4,3,3,3,3,3,3,4),(-16.3957559868666,
-15.9097905331194,-14.9154286247995,-13.9210667164795,-12.9267048081595,
-11.9323428998396,-10.9379809915196,-10.1125706796871),.UNSPECIFIED.);
#1638=B_SPLINE_CURVE_WITH_KNOTS('',3,(#8526,#8527,#8528,#8529,#8530,#8531,
#8532,#8533,#8534,#8535,#8536,#8537,#8538),.UNSPECIFIED.,.F.,.F.,(4,3,3,
3,4),(-3.82938537250746,-2.98308572495989,-1.98872381663993,-0.994361908319963,
0.),.UNSPECIFIED.);
#1639=B_SPLINE_CURVE_WITH_KNOTS('',3,(#8541,#8542,#8543,#8544,#8545,#8546,
#8547,#8548,#8549,#8550,#8551,#8552,#8553,#8554,#8555,#8556,#8557,#8558,
#8559,#8560,#8561,#8562),.UNSPECIFIED.,.F.,.F.,(4,3,3,3,3,3,3,4),(1.76301298203565,
1.98872381663993,2.98308572495989,3.97744763327985,4.97180954159982,5.96617144991978,
6.96053335823975,7.35840557029759),.UNSPECIFIED.);
#1640=B_SPLINE_CURVE_WITH_KNOTS('',3,(#8568,#8569,#8570,#8571),
 .UNSPECIFIED.,.F.,.F.,(4,4),(122.522113490002,123.247111627277),
 .UNSPECIFIED.);
#1641=B_SPLINE_CURVE_WITH_KNOTS('',3,(#8574,#8575,#8576,#8577,#8578,#8579),
 .UNSPECIFIED.,.F.,.F.,(4,1,1,4),(122.522113490002,123.018191011707,124.012552920027,
124.238263754631),.UNSPECIFIED.);
#1642=B_SPLINE_CURVE_WITH_KNOTS('',3,(#8584,#8585,#8586,#8587,#8588,#8589,
#8590,#8591,#8592,#8593,#8594),.UNSPECIFIED.,.F.,.F.,(4,1,1,1,1,1,1,1,4),
(116.238928182822,116.286578269038,117.280940177358,118.275302085678,119.269663993997,
120.264025902317,121.258387810637,122.252749718957,122.522113490002),
 .UNSPECIFIED.);
#1643=B_SPLINE_CURVE_WITH_KNOTS('',3,(#8595,#8596,#8597,#8598,#8599,#8600,
#8601,#8602,#8603,#8604),.UNSPECIFIED.,.F.,.F.,(4,1,1,1,1,1,1,4),(116.238928182822,
117.052019561787,118.046381470107,119.040743378427,120.035105286747,121.029467195067,
122.023829103387,122.522113490002),.UNSPECIFIED.);
#1644=B_SPLINE_CURVE_WITH_KNOTS('',3,(#8609,#8610,#8611,#8612,#8613,#8614,
#8615,#8616,#8617,#8618),.UNSPECIFIED.,.F.,.F.,(4,1,1,1,1,1,1,4),(109.955742875643,
110.320406819118,111.314768727438,112.309130635758,113.303492544078,114.297854452398,
115.292216360718,116.238928182822),.UNSPECIFIED.);
#1645=B_SPLINE_CURVE_WITH_KNOTS('',3,(#8619,#8620,#8621,#8622,#8623,#8624,
#8625,#8626,#8627,#8628,#8629),.UNSPECIFIED.,.F.,.F.,(4,1,1,1,1,1,1,1,4),
(109.955742875643,110.091486203547,111.085848111867,112.080210020187,113.074571928507,
114.068933836827,115.063295745147,116.057657653467,116.238928182822),
 .UNSPECIFIED.);
#1646=B_SPLINE_CURVE_WITH_KNOTS('',3,(#8634,#8635,#8636,#8637,#8638,#8639,
#8640,#8641,#8642,#8643),.UNSPECIFIED.,.F.,.F.,(4,1,1,1,1,1,1,4),(103.672557568463,
104.354235369198,105.348597277518,106.342959185838,107.337321094158,108.331683002478,
109.326044910798,109.955742875643),.UNSPECIFIED.);
#1647=B_SPLINE_CURVE_WITH_KNOTS('',3,(#8644,#8645,#8646,#8647,#8648,#8649,
#8650,#8651,#8652,#8653),.UNSPECIFIED.,.F.,.F.,(4,1,1,1,1,1,1,4),(103.672557568463,
104.125314753628,105.119676661947,106.114038570267,107.108400478587,108.102762386907,
109.097124295227,109.955742875643),.UNSPECIFIED.);
#1648=B_SPLINE_CURVE_WITH_KNOTS('',3,(#8658,#8659,#8660,#8661,#8662,#8663,
#8664,#8665,#8666,#8667,#8668),.UNSPECIFIED.,.F.,.F.,(4,1,1,1,1,1,1,1,4),
(97.3893722612835,97.3937020109583,98.3880639192782,99.3824258275982,100.376787735918,
101.371149644238,102.365511552558,103.359873460878,103.672557568463),
 .UNSPECIFIED.);
#1649=B_SPLINE_CURVE_WITH_KNOTS('',3,(#8669,#8670,#8671,#8672,#8673,#8674,
#8675,#8676,#8677,#8678),.UNSPECIFIED.,.F.,.F.,(4,1,1,1,1,1,1,4),(97.3893722612835,
98.1591433037077,99.1535052120277,100.147867120348,101.142229028668,102.136590936988,
103.130952845308,103.672557568463),.UNSPECIFIED.);
#1650=B_SPLINE_CURVE_WITH_KNOTS('',3,(#8683,#8684,#8685,#8686,#8687,#8688,
#8689,#8690,#8691,#8692),.UNSPECIFIED.,.F.,.F.,(4,1,1,1,1,1,1,4),(91.106186954104,
91.4275305610385,92.4218924693585,93.4162543776784,94.4106162859984,95.4049781943183,
96.3993401026383,97.3893722612835),.UNSPECIFIED.);
#1651=B_SPLINE_CURVE_WITH_KNOTS('',3,(#8693,#8694,#8695,#8696,#8697,#8698,
#8699,#8700,#8701,#8702,#8703),.UNSPECIFIED.,.F.,.F.,(4,1,1,1,1,1,1,1,4),
(91.106186954104,91.198609945468,92.1929718537879,93.1873337621079,94.1816956704279,
95.1760575787478,96.1704194870678,97.1647813953878,97.3893722612835),
 .UNSPECIFIED.);
#1652=B_SPLINE_CURVE_WITH_KNOTS('',3,(#8708,#8709,#8710,#8711,#8712,#8713,
#8714,#8715,#8716,#8717),.UNSPECIFIED.,.F.,.F.,(4,1,1,1,1,1,1,4),(84.8230016469244,
85.4613591111187,86.4557210194387,87.4500829277586,88.4444448360786,89.4388067443986,
90.4331686527185,91.106186954104),.UNSPECIFIED.);
#1653=B_SPLINE_CURVE_WITH_KNOTS('',3,(#8718,#8719,#8720,#8721,#8722,#8723,
#8724,#8725,#8726,#8727),.UNSPECIFIED.,.F.,.F.,(4,1,1,1,1,1,1,4),(84.8230016469244,
85.2324384955482,86.2268004038682,87.2211623121881,88.2155242205081,89.209886128828,
90.204248037148,91.106186954104),.UNSPECIFIED.);
#1654=B_SPLINE_CURVE_WITH_KNOTS('',3,(#8732,#8733,#8734,#8735,#8736,#8737,
#8738,#8739,#8740,#8741),.UNSPECIFIED.,.F.,.F.,(4,1,1,1,1,1,1,4),(78.5398163397447,
79.4951876611989,80.4895495695189,81.4839114778388,82.4782733861588,83.4726352944788,
84.4669972027987,84.8230016469244),.UNSPECIFIED.);
#1655=B_SPLINE_CURVE_WITH_KNOTS('',3,(#8742,#8743,#8744,#8745,#8746,#8747,
#8748,#8749,#8750,#8751),.UNSPECIFIED.,.F.,.F.,(4,1,1,1,1,1,1,4),(78.5398163397447,
79.2662670456284,80.2606289539484,81.2549908622683,82.2493527705883,83.2437146789083,
84.2380765872282,84.8230016469244),.UNSPECIFIED.);
#1656=B_SPLINE_CURVE_WITH_KNOTS('',3,(#8756,#8757,#8758,#8759,#8760,#8761,
#8762,#8763,#8764,#8765,#8766),.UNSPECIFIED.,.F.,.F.,(4,1,1,1,1,1,1,1,4),
(72.2566310325652,72.5346543029592,73.5290162112791,74.5233781195991,75.5177400279191,
76.512101936239,77.506463844559,78.500825752879,78.5398163397447),
 .UNSPECIFIED.);
#1657=B_SPLINE_CURVE_WITH_KNOTS('',3,(#8767,#8768,#8769,#8770,#8771,#8772,
#8773,#8774,#8775,#8776,#8777),.UNSPECIFIED.,.F.,.F.,(4,1,1,1,1,1,1,1,4),
(72.2566310325652,72.3057336873887,73.3000955957086,74.2944575040286,75.2888194123486,
76.2831813206685,77.2775432289885,78.2719051373085,78.5398163397447),
 .UNSPECIFIED.);
#1658=B_SPLINE_CURVE_WITH_KNOTS('',3,(#8782,#8783,#8784,#8785,#8786,#8787,
#8788,#8789,#8790,#8791),.UNSPECIFIED.,.F.,.F.,(4,1,1,1,1,1,1,4),(65.9734457253856,
66.5684828530394,67.5628447613594,68.5572066696793,69.5515685779993,70.5459304863193,
71.5402923946392,72.2566310325652),.UNSPECIFIED.);
#1659=B_SPLINE_CURVE_WITH_KNOTS('',3,(#8792,#8793,#8794,#8795,#8796,#8797,
#8798,#8799,#8800,#8801),.UNSPECIFIED.,.F.,.F.,(4,1,1,1,1,1,1,4),(65.9734457253856,
66.3395622374689,67.3339241457888,68.3282860541088,69.3226479624288,70.3170098707487,
71.3113717790687,72.2566310325652),.UNSPECIFIED.);
#1660=B_SPLINE_CURVE_WITH_KNOTS('',3,(#8806,#8807,#8808,#8809,#8810,#8811,
#8812,#8813,#8814,#8815),.UNSPECIFIED.,.F.,.F.,(4,1,1,1,1,1,1,4),(59.690260418206,
60.6023114031196,61.5966733114396,62.5910352197595,63.5853971280795,64.5797590363995,
65.5741209447194,65.9734457253856),.UNSPECIFIED.);
#1661=B_SPLINE_CURVE_WITH_KNOTS('',3,(#8816,#8817,#8818,#8819,#8820,#8821,
#8822,#8823,#8824,#8825),.UNSPECIFIED.,.F.,.F.,(4,1,1,1,1,1,1,4),(59.690260418206,
60.3733907875491,61.3677526958691,62.362114604189,63.356476512509,64.350838420829,
65.3452003291489,65.9734457253856),.UNSPECIFIED.);
#1662=B_SPLINE_CURVE_WITH_KNOTS('',3,(#8830,#8831,#8832,#8833,#8834,#8835,
#8836,#8837,#8838,#8839,#8840),.UNSPECIFIED.,.F.,.F.,(4,1,1,1,1,1,1,1,4),
(53.4070751110264,53.6417780448799,54.6361399531998,55.6305018615198,56.6248637698398,
57.6192256781597,58.6135875864797,59.6079494947996,59.690260418206),
 .UNSPECIFIED.);
#1663=B_SPLINE_CURVE_WITH_KNOTS('',3,(#8841,#8842,#8843,#8844,#8845,#8846,
#8847,#8848,#8849,#8850,#8851),.UNSPECIFIED.,.F.,.F.,(4,1,1,1,1,1,1,1,4),
(53.4070751110264,53.4128574293094,54.4072193376293,55.4015812459493,56.3959431542693,
57.3903050625892,58.3846669709092,59.3790288792291,59.690260418206),
 .UNSPECIFIED.);
#1664=B_SPLINE_CURVE_WITH_KNOTS('',3,(#8856,#8857,#8858,#8859,#8860,#8861,
#8862,#8863,#8864,#8865),.UNSPECIFIED.,.F.,.F.,(4,1,1,1,1,1,1,4),(47.1238898038468,
47.6756065949601,48.6699685032801,49.6643304116,50.65869231992,51.6530542282399,
52.6474161365599,53.4070751110264),.UNSPECIFIED.);
#1665=B_SPLINE_CURVE_WITH_KNOTS('',3,(#8866,#8867,#8868,#8869,#8870,#8871,
#8872,#8873,#8874,#8875),.UNSPECIFIED.,.F.,.F.,(4,1,1,1,1,1,1,4),(47.1238898038468,
47.4466859793896,48.4410478877095,49.4354097960295,50.4297717043495,51.4241336126694,
52.4184955209894,53.4070751110264),.UNSPECIFIED.);
#1666=B_SPLINE_CURVE_WITH_KNOTS('',3,(#8880,#8881,#8882,#8883,#8884,#8885,
#8886,#8887,#8888,#8889),.UNSPECIFIED.,.F.,.F.,(4,1,1,1,1,1,1,4),(40.8407044966672,
41.7094351450403,42.7037970533603,43.6981589616802,44.6925208700002,45.6868827783202,
46.6812446866401,47.1238898038468),.UNSPECIFIED.);
#1667=B_SPLINE_CURVE_WITH_KNOTS('',3,(#8890,#8891,#8892,#8893,#8894,#8895,
#8896,#8897,#8898,#8899),.UNSPECIFIED.,.F.,.F.,(4,1,1,1,1,1,1,4),(40.8407044966672,
41.4805145294698,42.4748764377898,43.4692383461097,44.4636002544297,45.4579621627497,
46.4523240710696,47.1238898038468),.UNSPECIFIED.);
#1668=B_SPLINE_CURVE_WITH_KNOTS('',3,(#8904,#8905,#8906,#8907,#8908,#8909,
#8910,#8911,#8912,#8913,#8914),.UNSPECIFIED.,.F.,.F.,(4,1,1,1,1,1,1,1,4),
(34.5575191894876,34.7489017868006,35.7432636951205,36.7376256034405,37.7319875117605,
38.7263494200804,39.7207113284004,40.7150732367203,40.8407044966672),
 .UNSPECIFIED.);
#1669=B_SPLINE_CURVE_WITH_KNOTS('',3,(#8915,#8916,#8917,#8918,#8919,#8920,
#8921,#8922,#8923,#8924),.UNSPECIFIED.,.F.,.F.,(4,1,1,1,1,1,1,4),(34.5575191894876,
35.51434307955,36.50870498787,37.5030668961899,38.4974288045099,39.4917907128299,
40.4861526211498,40.8407044966672),.UNSPECIFIED.);
#1670=B_SPLINE_CURVE_WITH_KNOTS('',3,(#8929,#8930,#8931,#8932,#8933,#8934,
#8935,#8936,#8937,#8938),.UNSPECIFIED.,.F.,.F.,(4,1,1,1,1,1,1,4),(28.274333882308,
28.7827303368808,29.7770922452007,30.7714541535207,31.7658160618407,32.7601779701606,
33.7545398784806,34.5575191894876),.UNSPECIFIED.);
#1671=B_SPLINE_CURVE_WITH_KNOTS('',3,(#8939,#8940,#8941,#8942,#8943,#8944,
#8945,#8946,#8947,#8948,#8949),.UNSPECIFIED.,.F.,.F.,(4,1,1,1,1,1,1,1,4),
(28.274333882308,28.5538097213103,29.5481716296302,30.5425335379502,31.5368954462702,
32.5312573545901,33.5256192629101,34.5199811712301,34.5575191894876),
 .UNSPECIFIED.);
#1672=B_SPLINE_CURVE_WITH_KNOTS('',3,(#8954,#8955,#8956,#8957,#8958,#8959,
#8960,#8961,#8962,#8963),.UNSPECIFIED.,.F.,.F.,(4,1,1,1,1,1,1,4),(21.9911485751284,
22.816558886961,23.810920795281,24.8052827036009,25.7996446119209,26.7940065202408,
27.7883684285608,28.274333882308),.UNSPECIFIED.);
#1673=B_SPLINE_CURVE_WITH_KNOTS('',3,(#8964,#8965,#8966,#8967,#8968,#8969,
#8970,#8971,#8972,#8973),.UNSPECIFIED.,.F.,.F.,(4,1,1,1,1,1,1,4),(21.9911485751284,
22.5876382713905,23.5820001797105,24.5763620880304,25.5707239963504,26.5650859046703,
27.5594478129903,28.274333882308),.UNSPECIFIED.);
#1674=B_SPLINE_CURVE_WITH_KNOTS('',3,(#8979,#8980,#8981,#8982,#8983),
 .UNSPECIFIED.,.F.,.F.,(4,1,4),(14.6327430048308,15.6271049131507,15.7079632679489),
 .UNSPECIFIED.);
#1675=B_SPLINE_CURVE_WITH_KNOTS('',3,(#8986,#8987,#8988,#8989,#8990,#8991),
 .UNSPECIFIED.,.F.,.F.,(4,1,1,4),(13.6415908774771,13.8673017120813,14.8616636204013,
15.7079632679489),.UNSPECIFIED.);
#1676=B_SPLINE_CURVE_WITH_KNOTS('',3,(#8996,#8997,#8998,#8999,#9000,#9001,
#9002,#9003,#9004,#9005,#9006,#9007,#9008,#9009,#9010,#9011,#9012,#9013,
#9014,#9015,#9016,#9017,#9018,#9019,#9020,#9021,#9022,#9023,#9024,#9025,
#9026,#9027,#9028,#9029,#9030,#9031,#9032,#9033,#9034,#9035,#9036,#9037,
#9038,#9039,#9040,#9041,#9042,#9043,#9044,#9045,#9046,#9047,#9048,#9049,
#9050,#9051,#9052,#9053,#9054,#9055,#9056,#9057,#9058,#9059,#9060,#9061,
#9062,#9063,#9064,#9065,#9066,#9067,#9068,#9069,#9070,#9071,#9072,#9073,
#9074,#9075,#9076,#9077),.UNSPECIFIED.,.F.,.F.,(4,3,3,3,3,3,3,3,3,3,3,3,
3,3,3,3,3,3,3,3,3,3,3,3,3,3,3,4),(-0.659098020064273,-0.626583361418082,
-0.593277974374451,-0.55935451242369,-0.553527494448718,-0.547862782208884,
-0.513423105891954,-0.478559830537098,-0.456043474192613,-0.446497663053644,
-0.441032459037381,-0.405381589223341,-0.36977595468836,-0.334102467234791,
-0.316265723508006,-0.30668221639439,-0.301163149286353,-0.298428979781222,
-0.2643597751017,-0.228954386588656,-0.19290020592246,-0.168787680182153,
-0.157455049850378,-0.152068965805326,-0.114051724353995,-0.076872177317131,
-0.0384360886585655,0.),.UNSPECIFIED.);
#1677=B_SPLINE_CURVE_WITH_KNOTS('',3,(#9078,#9079,#9080,#9081,#9082,#9083,
#9084,#9085,#9086,#9087,#9088,#9089,#9090,#9091,#9092,#9093,#9094,#9095,
#9096,#9097,#9098,#9099,#9100,#9101,#9102,#9103,#9104,#9105,#9106,#9107,
#9108,#9109,#9110,#9111,#9112,#9113,#9114,#9115,#9116,#9117,#9118,#9119,
#9120,#9121,#9122,#9123,#9124,#9125,#9126,#9127,#9128,#9129,#9130,#9131,
#9132,#9133,#9134,#9135,#9136,#9137,#9138,#9139,#9140,#9141,#9142,#9143,
#9144,#9145,#9146,#9147,#9148,#9149,#9150,#9151,#9152,#9153,#9154,#9155,
#9156,#9157,#9158,#9159),.UNSPECIFIED.,.F.,.F.,(4,3,3,3,3,3,3,3,3,3,3,3,
3,3,3,3,3,3,3,3,3,3,3,3,3,3,3,4),(-0.657201022293968,-0.620843507912061,
-0.583812069642265,-0.545304753610891,-0.539298492849628,-0.533288478909317,
-0.49669576643024,-0.460284093722029,-0.437217774680684,-0.425131515458518,
-0.419071806367675,-0.383242240123574,-0.34808971350986,-0.311921627450565,
-0.293837584420918,-0.284384662265536,-0.278693413802068,-0.27575354139127,
-0.241284348717361,-0.206301309944578,-0.171212377127033,-0.149810829986154,
-0.13853214715148,-0.133449179146389,-0.0991640919442515,-0.0650684826066501,
-0.0318743752082536,0.),.UNSPECIFIED.);
#1678=B_SPLINE_CURVE_WITH_KNOTS('',3,(#9161,#9162,#9163,#9164,#9165,#9166,
#9167,#9168,#9169,#9170,#9171),.UNSPECIFIED.,.F.,.F.,(4,1,1,1,1,1,1,1,4),
(15.7079632679489,15.8560255287213,16.8503874370412,17.8447493453612,18.8391112536811,
19.8334731620011,20.8278350703211,21.822196978641,21.9911485751284),
 .UNSPECIFIED.);
#1679=B_SPLINE_CURVE_WITH_KNOTS('',3,(#9172,#9173,#9174,#9175,#9176,#9177,
#9178,#9179,#9180,#9181),.UNSPECIFIED.,.F.,.F.,(4,1,1,1,1,1,1,4),(15.7079632679489,
16.6214668214707,17.6158287297907,18.6101906381106,19.6045525464306,20.5989144547506,
21.5932763630705,21.9911485751284),.UNSPECIFIED.);
#1680=B_SPLINE_CURVE_WITH_KNOTS('',3,(#9642,#9643,#9644,#9645,#9646,#9647,
#9648,#9649,#9650,#9651,#9652,#9653,#9654,#9655,#9656,#9657,#9658,#9659,
#9660,#9661,#9662,#9663,#9664,#9665,#9666,#9667,#9668,#9669,#9670,#9671,
#9672,#9673,#9674,#9675,#9676,#9677,#9678,#9679,#9680,#9681,#9682,#9683,
#9684,#9685,#9686,#9687,#9688,#9689,#9690,#9691,#9692,#9693,#9694,#9695,
#9696,#9697,#9698,#9699,#9700,#9701,#9702,#9703,#9704,#9705,#9706,#9707,
#9708,#9709,#9710,#9711,#9712,#9713,#9714,#9715,#9716,#9717,#9718,#9719,
#9720,#9721,#9722,#9723),.UNSPECIFIED.,.F.,.F.,(4,3,3,3,3,3,3,3,3,3,3,3,
3,3,3,3,3,3,3,3,3,3,3,3,3,3,3,4),(-0.659098020064319,-0.626583355717508,
-0.593277963850765,-0.559354498782614,-0.553527466898513,-0.547862778460467,
-0.513423098595221,-0.478559821819824,-0.456043466564999,-0.446497640120997,
-0.441032457407506,-0.405381588000935,-0.369775954373192,-0.334102467077208,
-0.316265723429216,-0.306682216314082,-0.301163149097039,-0.298428979781224,
-0.264359779778512,-0.22895439423595,-0.192900215169359,-0.168787688273189,
-0.157455061634061,-0.152068971468546,-0.114051728601409,-0.0768721821854325,
-0.0384360910927163,0.),.UNSPECIFIED.);
#1681=B_SPLINE_CURVE_WITH_KNOTS('',3,(#9724,#9725,#9726,#9727,#9728,#9729,
#9730,#9731,#9732,#9733,#9734,#9735,#9736,#9737,#9738,#9739,#9740,#9741,
#9742,#9743,#9744,#9745,#9746,#9747,#9748),.UNSPECIFIED.,.F.,.F.,(4,3,3,
3,3,3,3,3,4),(-10.1125706796871,-9.94361908319964,-8.94925717487967,-7.95489526655971,
-6.96053335823974,-5.96617144991978,-4.97180954159982,-3.97744763327986,
-3.82938537250746),.UNSPECIFIED.);
#1682=B_SPLINE_CURVE_WITH_KNOTS('',3,(#9750,#9751,#9752,#9753,#9754,#9755,
#9756,#9757,#9758,#9759,#9760,#9761,#9762,#9763,#9764,#9765,#9766,#9767,
#9768,#9769,#9770,#9771,#9772,#9773,#9774,#9775,#9776,#9777,#9778,#9779,
#9780,#9781,#9782,#9783,#9784,#9785,#9786,#9787,#9788,#9789,#9790,#9791,
#9792,#9793,#9794,#9795,#9796,#9797,#9798,#9799,#9800,#9801,#9802,#9803,
#9804,#9805,#9806,#9807,#9808,#9809,#9810,#9811,#9812,#9813,#9814,#9815,
#9816,#9817,#9818,#9819,#9820,#9821,#9822,#9823,#9824,#9825,#9826,#9827,
#9828,#9829,#9830,#9831),.UNSPECIFIED.,.F.,.F.,(4,3,3,3,3,3,3,3,3,3,3,3,
3,3,3,3,3,3,3,3,3,3,3,3,3,3,3,4),(-0.657201022293926,-0.620843512226781,
-0.583812075977012,-0.545304759153794,-0.539298504171762,-0.533288480271845,
-0.496695767933232,-0.460284093901184,-0.437217774837445,-0.425131516019463,
-0.419071806729443,-0.3832422403949,-0.348089712058185,-0.311921626724727,
-0.293837584057999,-0.284384661973879,-0.278693413430814,-0.27575354139127,
-0.241284348717361,-0.206301309906783,-0.171212377154442,-0.149810830010137,
-0.138532146710759,-0.133449178888522,-0.0991640917928147,-0.0650684819880444,
-0.0318743724222816,0.),.UNSPECIFIED.);
#1683=B_SPLINE_CURVE_WITH_KNOTS('',3,(#10295,#10296,#10297,#10298,#10299,
#10300,#10301,#10302,#10303,#10304,#10305,#10306,#10307,#10308,#10309,#10310,
#10311,#10312,#10313,#10314,#10315,#10316),.UNSPECIFIED.,.F.,.F.,(4,3,3,
3,3,3,3,4),(7.35840557029759,7.95489526655971,8.94925717487967,9.94361908319964,
10.9379809915196,11.9323428998396,12.9267048081595,13.6415908774772),
 .UNSPECIFIED.);
#1684=B_SPLINE_CURVE_WITH_KNOTS('',3,(#10431,#10432,#10433,#10434,#10435),
 .UNSPECIFIED.,.F.,.F.,(4,1,4),(0.,0.5,1.),.UNSPECIFIED.);
#1685=B_SPLINE_CURVE_WITH_KNOTS('',3,(#10439,#10440,#10441,#10442,#10443),
 .UNSPECIFIED.,.F.,.F.,(4,1,4),(0.,0.5,1.),.UNSPECIFIED.);
#1686=B_SPLINE_CURVE_WITH_KNOTS('',3,(#10466,#10467,#10468,#10469),
 .UNSPECIFIED.,.F.,.F.,(4,4),(0.088693979487329,0.125274232772668),
 .UNSPECIFIED.);
#1687=B_SPLINE_CURVE_WITH_KNOTS('',3,(#10472,#10473,#10474,#10475),
 .UNSPECIFIED.,.F.,.F.,(4,4),(-0.125274232772668,-0.088693979487329),
 .UNSPECIFIED.);
#1688=B_SPLINE_CURVE_WITH_KNOTS('',3,(#10485,#10486,#10487,#10488,#10489,
#10490,#10491,#10492,#10493,#10494,#10495,#10496,#10497,#10498,#10499,#10500,
#10501,#10502,#10503,#10504,#10505),.UNSPECIFIED.,.F.,.F.,(4,1,1,1,1,1,
1,1,1,1,1,1,1,1,1,1,1,1,4),(0.,2.5201892997592,5.0403785995184,6.72050479935786,
8.40063099919733,10.0807571990368,11.7608833988763,15.1211357985552,15.9611988984749,
16.8012619983947,20.1615143980736,21.841640597913,23.5217667977525,25.201892997592,
26.8820191974314,28.5621453972709,30.2422715971104,32.7624608968696,35.2826501966288),
 .UNSPECIFIED.);
#1689=B_SPLINE_CURVE_WITH_KNOTS('',3,(#10597,#10598,#10599,#10600,#10601,
#10602,#10603,#10604,#10605,#10606,#10607,#10608,#10609,#10610,#10611,#10612,
#10613,#10614,#10615,#10616,#10617,#10618),.UNSPECIFIED.,.F.,.F.,(4,1,1,
1,1,1,1,1,1,1,1,1,1,1,1,1,1,1,1,4),(-34.8725995211214,-32.381699555327,
-29.8907995895326,-28.2301996123364,-26.5695996351401,-24.9089996579439,
-23.2483996807476,-21.5877997035514,-19.9271997263551,-18.2665997491588,
-16.6059997719626,-14.9453997947663,-13.2847998175701,-11.6241998403738,
-9.96359986317755,-8.30299988598129,-6.64239990878503,-4.98179993158877,
-2.49089996579439,0.),.UNSPECIFIED.);
#1690=B_SPLINE_CURVE_WITH_KNOTS('',3,(#10621,#10622,#10623,#10624,#10625,
#10626,#10627,#10628,#10629,#10630,#10631,#10632,#10633,#10634,#10635,#10636,
#10637,#10638,#10639,#10640,#10641,#10642),.UNSPECIFIED.,.F.,.F.,(4,1,1,
1,1,1,1,1,1,1,1,1,1,1,1,1,1,1,1,4),(0.,2.49089996579439,4.98179993158877,
6.64239990878503,8.30299988598129,9.96359986317755,11.6241998403738,13.2847998175701,
14.9453997947663,16.6059997719626,18.2665997491588,19.9271997263551,21.5877997035514,
23.2483996807476,24.9089996579439,26.5695996351401,28.2301996123364,29.8907995895326,
32.381699555327,34.8725995211214),.UNSPECIFIED.);
#1691=B_SPLINE_CURVE_WITH_KNOTS('',3,(#10669,#10670,#10671,#10672),
 .UNSPECIFIED.,.F.,.F.,(4,4),(0.0886939794873267,0.125274232772633),
 .UNSPECIFIED.);
#1692=B_SPLINE_CURVE_WITH_KNOTS('',3,(#10673,#10674,#10675,#10676),
 .UNSPECIFIED.,.F.,.F.,(4,4),(-0.125274232772633,-0.0886939794873267),
 .UNSPECIFIED.);
#1693=B_SPLINE_CURVE_WITH_KNOTS('',3,(#10694,#10695,#10696,#10697),
 .UNSPECIFIED.,.F.,.F.,(4,4),(-0.860462555942468,-0.587131769179142),
 .UNSPECIFIED.);
#1694=B_SPLINE_CURVE_WITH_KNOTS('',3,(#10699,#10700,#10701,#10702,#10703,
#10704,#10705,#10706,#10707,#10708,#10709,#10710,#10711,#10712,#10713,#10714,
#10715,#10716,#10717,#10718,#10719,#10720,#10721,#10722,#10723),
 .UNSPECIFIED.,.F.,.F.,(4,3,3,3,3,3,3,3,4),(-0.000295685355657064,0.,0.010783911952954,
0.021297945774393,0.0312974952251527,0.034783930866502,0.0432659714995236,
0.0512040825193111,0.0584686894100284),.UNSPECIFIED.);
#1695=B_SPLINE_CURVE_WITH_KNOTS('',3,(#10725,#10726,#10727,#10728,#10729,
#10730),.UNSPECIFIED.,.F.,.F.,(4,2,4),(-0.0365164375971617,-0.026613618341596,
0.),.UNSPECIFIED.);
#1696=B_SPLINE_CURVE_WITH_KNOTS('',3,(#10731,#10732,#10733,#10734),
 .UNSPECIFIED.,.F.,.F.,(4,4),(0.649033397962949,0.860462555942468),
 .UNSPECIFIED.);
#1697=B_SPLINE_CURVE_WITH_KNOTS('',3,(#10916,#10917,#10918,#10919),
 .UNSPECIFIED.,.F.,.F.,(4,4),(-0.292336438831091,-0.0190073922957582),
 .UNSPECIFIED.);
#1698=B_SPLINE_CURVE_WITH_KNOTS('',3,(#10921,#10922,#10923,#10924),
 .UNSPECIFIED.,.F.,.F.,(4,4),(-34.9074997830359,-34.6574150541607),
 .UNSPECIFIED.);
#1699=B_SPLINE_CURVE_WITH_KNOTS('',3,(#10941,#10942,#10943,#10944,#10945,
#10946,#10947,#10948,#10949,#10950,#10951,#10952,#10953,#10954,#10955,#10956,
#10957,#10958,#10959,#10960,#10961,#10962,#10963),.UNSPECIFIED.,.T.,.F.,
(4,1,1,1,1,1,1,1,1,1,1,1,1,1,1,1,1,1,1,1,4),(-7.85398163397448,-7.40518268346166,
-6.95638373294883,-6.65718443260694,-6.35798513226506,-6.20838548209412,
-6.05878583192317,-5.75958653158129,-5.4603872312394,-5.16118793089752,
-4.86198863055563,-4.56278933021375,-4.26359002987186,-3.96439072952998,
-3.66519142918809,-3.36599212884621,-3.06679282850432,-2.76759352816244,
-2.46839422782055,-2.01959527730772,-1.5707963267949),.UNSPECIFIED.);
#1700=B_SPLINE_CURVE_WITH_KNOTS('',3,(#10964,#10965,#10966,#10967),
 .UNSPECIFIED.,.F.,.F.,(4,4),(-35.1575805274809,-34.9074997830359),
 .UNSPECIFIED.);
#1701=B_SPLINE_CURVE_WITH_KNOTS('',3,(#10985,#10986,#10987,#10988),
 .UNSPECIFIED.,.F.,.F.,(4,4),(0.0190073922957582,0.230436959265831),
 .UNSPECIFIED.);
#1702=B_SPLINE_CURVE_WITH_KNOTS('',3,(#10990,#10991,#10992,#10993,#10994,
#10995,#10996,#10997),.UNSPECIFIED.,.F.,.F.,(4,2,2,4),(-0.0846091546938526,
-0.070148598643786,-0.0557294988245446,-0.048303086999004),
 .UNSPECIFIED.);
#1703=B_SPLINE_CURVE_WITH_KNOTS('',3,(#10998,#10999,#11000,#11001,#11002,
#11003,#11004,#11005),.UNSPECIFIED.,.F.,.F.,(4,2,2,4),(-0.0583052907282766,
-0.0580119153510426,-0.0234997264609151,0.),.UNSPECIFIED.);
#1704=B_SPLINE_CURVE_WITH_KNOTS('',3,(#11008,#11009,#11010,#11011),
 .UNSPECIFIED.,.F.,.F.,(4,4),(0.875635390636623,1.1096475233552),
 .UNSPECIFIED.);
#1705=B_SPLINE_CURVE_WITH_KNOTS('',3,(#11108,#11109,#11110,#11111,#11112,
#11113,#11114,#11115,#11116,#11117,#11118,#11119,#11120),.UNSPECIFIED.,
 .F.,.F.,(4,1,1,1,1,1,1,1,1,1,4),(1.5707963267949,2.01959527730772,2.46839422782055,
2.76759352816244,3.06679282850432,3.36599212884621,3.66519142918809,3.96439072952998,
4.26359002987186,4.56278933021375,4.71238073889391),.UNSPECIFIED.);
#1706=B_SPLINE_CURVE_WITH_KNOTS('',3,(#11121,#11122,#11123,#11124,#11125,
#11126,#11127,#11128,#11129,#11130,#11131,#11132,#11133,#11134),
 .UNSPECIFIED.,.F.,.F.,(4,1,1,1,1,1,1,1,1,1,1,4),(4.71238073889391,4.86198863055563,
5.16118793089752,5.4603872312394,5.75958653158129,6.05878583192317,6.20838548209412,
6.35798513226506,6.65718443260694,6.95638373294883,7.40518268346166,7.85398163397448),
 .UNSPECIFIED.);
#1707=B_SPLINE_CURVE_WITH_KNOTS('',3,(#11351,#11352,#11353,#11354,#11355,
#11356,#11357,#11358,#11359,#11360,#11361,#11362,#11363,#11364,#11365,#11366,
#11367,#11368,#11369,#11370,#11371),.UNSPECIFIED.,.F.,.F.,(4,1,1,1,1,1,
1,1,1,1,1,1,1,1,1,1,1,1,4),(-35.2826501966288,-32.7624608968696,-30.2422715971104,
-28.5621453972709,-26.8820191974314,-25.201892997592,-23.5217667977525,
-21.841640597913,-20.1615143980736,-16.8012619983947,-15.9611988984749,
-15.1211357985552,-11.7608833988763,-10.0807571990368,-8.40063099919733,
-6.72050479935786,-5.0403785995184,-2.5201892997592,0.),.UNSPECIFIED.);
#1708=B_SPLINE_CURVE_WITH_KNOTS('',3,(#11398,#11399,#11400,#11401),
 .UNSPECIFIED.,.F.,.F.,(4,4),(-1.1096475233552,-0.825569897711632),
 .UNSPECIFIED.);
#1709=B_SPLINE_CURVE_WITH_KNOTS('',3,(#11403,#11404,#11405,#11406,#11407,
#11408,#11409,#11410,#11411,#11412,#11413,#11414,#11415,#11416),
 .UNSPECIFIED.,.F.,.F.,(4,2,2,2,2,2,4),(-0.0987748436415996,-0.0846442489344777,
-0.0686516240192571,-0.0476703451541984,-0.0244527973261725,0.,0.00045791775862737),
 .UNSPECIFIED.);
#1710=B_SPLINE_CURVE_WITH_KNOTS('',3,(#11417,#11418,#11419,#11420),
 .UNSPECIFIED.,.F.,.F.,(4,4),(-0.000473389988960978,0.),.UNSPECIFIED.);
#1711=B_SPLINE_CURVE_WITH_KNOTS('',3,(#11647,#11648,#11649,#11650),
 .UNSPECIFIED.,.F.,.F.,(4,4),(-0.317361133028268,-0.0332835073847237),
 .UNSPECIFIED.);
#1712=B_SPLINE_CURVE_WITH_KNOTS('',3,(#11652,#11653,#11654,#11655),
 .UNSPECIFIED.,.F.,.F.,(4,4),(-36.1074649321654,-35.8573857487427),
 .UNSPECIFIED.);
#1713=B_SPLINE_CURVE_WITH_KNOTS('',3,(#11675,#11676,#11677,#11678),
 .UNSPECIFIED.,.F.,.F.,(4,4),(-36.3575403182,-36.1074649321654),
 .UNSPECIFIED.);
#1714=B_SPLINE_CURVE_WITH_KNOTS('',3,(#11696,#11697,#11698,#11699),
 .UNSPECIFIED.,.F.,.F.,(4,4),(0.0332835073847237,0.267295640103291),
 .UNSPECIFIED.);
#1715=B_SPLINE_CURVE_WITH_KNOTS('',3,(#11701,#11702,#11703,#11704),
 .UNSPECIFIED.,.F.,.F.,(4,4),(-0.0809288342320163,-0.0804554916472578),
 .UNSPECIFIED.);
#1716=B_SPLINE_CURVE_WITH_KNOTS('',3,(#11705,#11706,#11707,#11708,#11709,
#11710,#11711,#11712,#11713,#11714,#11715,#11716,#11717,#11718),
 .UNSPECIFIED.,.F.,.F.,(4,2,2,2,2,2,4),(0.,0.0139873855694353,0.0298179302556126,
0.0505865704508789,0.0735688157275276,0.0977737916359578,0.0982270685416762),
 .UNSPECIFIED.);
#1717=B_SPLINE_CURVE_WITH_KNOTS('',3,(#11738,#11739,#11740,#11741),
 .UNSPECIFIED.,.F.,.F.,(4,4),(34.6979587163218,34.7074565752905),
 .UNSPECIFIED.);
#1718=B_SPLINE_CURVE_WITH_KNOTS('',3,(#11743,#11744,#11745,#11746),
 .UNSPECIFIED.,.F.,.F.,(4,4),(34.7074565752905,35.1075404676718),
 .UNSPECIFIED.);
#1719=B_SPLINE_CURVE_WITH_KNOTS('',3,(#11747,#11748,#11749,#11750),
 .UNSPECIFIED.,.F.,.F.,(4,4),(-35.1170380704337,-35.1075404676718),
 .UNSPECIFIED.);
#1720=B_SPLINE_CURVE_WITH_KNOTS('',3,(#11753,#11754,#11755,#11756),
 .UNSPECIFIED.,.F.,.F.,(4,4),(36.3075029101841,36.3075051513331),
 .UNSPECIFIED.);
#1721=B_SPLINE_CURVE_WITH_KNOTS('',3,(#11758,#11759,#11760,#11761),
 .UNSPECIFIED.,.F.,.F.,(4,4),(35.9074245478542,36.3075029101841),
 .UNSPECIFIED.);
#1722=B_SPLINE_CURVE_WITH_KNOTS('',3,(#11762,#11763,#11764,#11765),
 .UNSPECIFIED.,.F.,.F.,(4,4),(-35.9074245478542,-35.9074223066489),
 .UNSPECIFIED.);
#1723=B_SPLINE_CURVE_WITH_KNOTS('',3,(#11853,#11854,#11855,#11856),
 .UNSPECIFIED.,.F.,.F.,(4,4),(-0.0736302548927899,-0.0606102871491874),
 .UNSPECIFIED.);
#1724=B_SPLINE_CURVE_WITH_KNOTS('',3,(#11862,#11863,#11864,#11865),
 .UNSPECIFIED.,.F.,.F.,(4,4),(-0.0535503409172659,0.),.UNSPECIFIED.);
#1725=B_SPLINE_CURVE_WITH_KNOTS('',3,(#11867,#11868,#11869,#11870,#11871,
#11872,#11873,#11874,#11875,#11876,#11877,#11878,#11879,#11880,#11881,#11882,
#11883,#11884,#11885,#11886,#11887,#11888,#11889,#11890,#11891,#11892,#11893,
#11894),.UNSPECIFIED.,.F.,.F.,(4,3,3,3,3,3,3,3,3,4),(-0.0707543141709639,
-0.0639700558869814,-0.0618906129072222,-0.0551601393419019,-0.0506565173110961,
-0.0464091777054624,-0.039691133709109,-0.0329985150203425,-0.0311186796527011,
-0.0241191350787041),.UNSPECIFIED.);
#1726=B_SPLINE_CURVE_WITH_KNOTS('',3,(#11896,#11897,#11898,#11899),
 .UNSPECIFIED.,.F.,.F.,(4,4),(0.,0.00710537445304894),.UNSPECIFIED.);
#1727=B_SPLINE_CURVE_WITH_KNOTS('',3,(#11903,#11904,#11905,#11906,#11907,
#11908,#11909,#11910,#11911,#11912,#11913,#11914,#11915,#11916,#11917,#11918,
#11919,#11920,#11921,#11922,#11923,#11924,#11925,#11926,#11927,#11928,#11929,
#11930,#11931,#11932,#11933,#11934,#11935,#11936,#11937,#11938,#11939,#11940,
#11941,#11942,#11943,#11944,#11945),.UNSPECIFIED.,.F.,.F.,(4,3,3,3,3,3,
3,3,3,3,3,3,3,3,4),(0.,0.00580629857172819,0.011668120368983,0.0175829585474277,
0.0201349204647166,0.0268347020686461,0.0295682026475181,0.0365019513209761,
0.0408129765218727,0.0451592379215555,0.0520962433453293,0.0563360701356979,
0.0584849555420972,0.0655164894020243,0.0715864535936182),.UNSPECIFIED.);
#1728=B_SPLINE_CURVE_WITH_KNOTS('',3,(#12040,#12041,#12042,#12043,#12044,
#12045,#12046,#12047,#12048,#12049,#12050,#12051,#12052,#12053,#12054,#12055,
#12056,#12057,#12058,#12059,#12060,#12061,#12062,#12063,#12064,#12065,#12066,
#12067,#12068,#12069,#12070,#12071,#12072,#12073,#12074,#12075,#12076,#12077,
#12078,#12079,#12080,#12081,#12082,#12083,#12084,#12085),.UNSPECIFIED.,
 .F.,.F.,(4,3,3,3,3,3,3,3,3,3,3,3,3,3,3,4),(0.,0.00694526795998421,0.0139543072598735,
0.015291136260988,0.0172103975930811,0.0240884241491964,0.0308533616756733,
0.0340363892002112,0.0409613583285485,0.0476241304298719,0.0499527776364528,
0.0515655803640436,0.0584478624259065,0.0609496822139948,0.0675796538345217,
0.0717651027806449),.UNSPECIFIED.);
#1729=B_SPLINE_CURVE_WITH_KNOTS('',3,(#12086,#12087,#12088,#12089,#12090,
#12091,#12092,#12093,#12094,#12095,#12096,#12097,#12098),.UNSPECIFIED.,
 .F.,.F.,(4,1,1,1,1,1,1,1,1,1,4),(-0.0122547872558393,0.0623967058774603,
0.13704819901076,0.211699692144059,0.267688311994034,0.286351185277359,
0.305014058560684,0.323676931844009,0.361002678410658,0.435654171543958,
0.510305664677257),.UNSPECIFIED.);
#1730=B_SPLINE_CURVE_WITH_KNOTS('',3,(#12099,#12100,#12101,#12102,#12103,
#12104,#12105,#12106,#12107,#12108,#12109,#12110,#12111,#12112,#12113,#12114,
#12115,#12116,#12117,#12118,#12119,#12120,#12121,#12122,#12123,#12124,#12125,
#12126,#12127,#12128,#12129),.UNSPECIFIED.,.F.,.F.,(4,3,3,3,3,3,3,3,3,3,
4),(0.000383354128218201,0.0625597845796719,0.136949375128678,0.174144170403181,
0.192741568040432,0.211338965677684,0.229936363314935,0.28572855622669,
0.360118146775696,0.434507737324702,0.496685534539592),.UNSPECIFIED.);
#1731=B_SPLINE_CURVE_WITH_KNOTS('',3,(#12163,#12164,#12165,#12166),
 .UNSPECIFIED.,.F.,.F.,(4,4),(-0.00710537445449871,0.),.UNSPECIFIED.);
#1732=B_SPLINE_CURVE_WITH_KNOTS('',3,(#12168,#12169,#12170,#12171),
 .UNSPECIFIED.,.F.,.F.,(4,4),(-0.0196379557516152,-0.000110621155015422),
 .UNSPECIFIED.);
#1733=B_SPLINE_CURVE_WITH_KNOTS('',3,(#12173,#12174,#12175,#12176,#12177,
#12178,#12179,#12180,#12181,#12182,#12183,#12184,#12185,#12186,#12187,#12188,
#12189,#12190,#12191,#12192,#12193,#12194,#12195,#12196,#12197),
 .UNSPECIFIED.,.F.,.F.,(4,3,3,3,3,3,3,3,4),(-0.0420242349144714,-0.034244024011145,
-0.0304445564291344,-0.0224018409775603,-0.0210691966450077,-0.0115168785817897,
-0.00144892293139089,0.,0.000288034171025875),.UNSPECIFIED.);
#1734=B_SPLINE_CURVE_WITH_KNOTS('',3,(#12201,#12202,#12203,#12204,#12205,
#12206,#12207,#12208,#12209,#12210,#12211,#12212,#12213,#12214,#12215,#12216,
#12217,#12218,#12219,#12220,#12221,#12222,#12223,#12224,#12225),
 .UNSPECIFIED.,.F.,.F.,(4,3,3,3,3,3,3,3,4),(-0.0422600918508368,-0.0419734950304658,
-0.0314914666110231,-0.021986817507206,-0.0210094381915805,-0.01300685760943,
-0.0116808634569233,-0.00393947746920935,-0.000158970042657082),
 .UNSPECIFIED.);
#1735=B_SPLINE_CURVE_WITH_KNOTS('',3,(#12226,#12227,#12228,#12229),
 .UNSPECIFIED.,.F.,.F.,(4,4),(-0.328977585058273,-0.317010469451376),
 .UNSPECIFIED.);
#1736=B_SPLINE_CURVE_WITH_KNOTS('',3,(#12232,#12233,#12234,#12235),
 .UNSPECIFIED.,.F.,.F.,(4,4),(0.,0.0383467777019652),.UNSPECIFIED.);
#1737=B_SPLINE_CURVE_WITH_KNOTS('',3,(#12238,#12239,#12240,#12241),
 .UNSPECIFIED.,.F.,.F.,(4,4),(0.127361965791744,0.165708743493706),
 .UNSPECIFIED.);
#1738=B_SPLINE_CURVE_WITH_KNOTS('',3,(#12266,#12267,#12268,#12269,#12270,
#12271,#12272,#12273,#12274,#12275,#12276,#12277,#12278,#12279,#12280,#12281,
#12282,#12283,#12284,#12285,#12286,#12287,#12288,#12289,#12290,#12291,#12292,
#12293),.UNSPECIFIED.,.F.,.F.,(4,3,3,3,3,3,3,3,3,4),(-0.103312994452742,
-0.0944972367595641,-0.0896726356037232,-0.081979706066035,-0.0758675452743191,
-0.0681010871890584,-0.0620124392214268,-0.0585654250906251,-0.0490657070288485,
-0.0435218377980582),.UNSPECIFIED.);
#1739=B_SPLINE_CURVE_WITH_KNOTS('',3,(#12336,#12337,#12338,#12339,#12340,
#12341,#12342,#12343,#12344,#12345,#12346,#12347,#12348,#12349,#12350,#12351,
#12352,#12353,#12354,#12355,#12356,#12357,#12358,#12359,#12360,#12361,#12362,
#12363,#12364,#12365,#12366),.UNSPECIFIED.,.F.,.F.,(4,3,3,3,3,3,3,3,3,3,
4),(-0.0462738036441523,-0.0389589150096727,-0.0346312122739206,-0.0286583377057116,
-0.0230059035179827,-0.0212406883770576,-0.0202962772284038,-0.014379131563933,
-0.0105565993757205,-0.00393990817803328,0.),.UNSPECIFIED.);
#1740=B_SPLINE_CURVE_WITH_KNOTS('',3,(#12367,#12368,#12369,#12370,#12371,
#12372,#12373,#12374,#12375,#12376,#12377,#12378,#12379,#12380,#12381,#12382,
#12383,#12384,#12385,#12386,#12387,#12388,#12389,#12390,#12391,#12392,#12393,
#12394),.UNSPECIFIED.,.F.,.F.,(4,3,3,3,3,3,3,3,3,4),(-0.070410764499354,
-0.0637409419809624,-0.0570604470106178,-0.0503274465588287,-0.0483425491955468,
-0.0438577936617308,-0.0371215088649918,-0.0325914562918353,-0.0258040649471257,
-0.023746438679814),.UNSPECIFIED.);
#1741=B_SPLINE_CURVE_WITH_KNOTS('',3,(#12421,#12422,#12423,#12424),
 .UNSPECIFIED.,.F.,.F.,(4,4),(-0.165708743493706,-0.112158402576443),
 .UNSPECIFIED.);
#1742=B_SPLINE_CURVE_WITH_KNOTS('',3,(#12442,#12443,#12444,#12445),
 .UNSPECIFIED.,.F.,.F.,(4,4),(-0.182084709739034,-0.169064741995431),
 .UNSPECIFIED.);
#1743=B_SPLINE_CURVE_WITH_KNOTS('',3,(#12494,#12495,#12496,#12497,#12498,
#12499,#12500,#12501,#12502,#12503),.UNSPECIFIED.,.F.,.F.,(4,2,2,2,4),(-0.000394703056647228,
0.,0.0306355392027269,0.0540522668896819,0.0684604040501524),
 .UNSPECIFIED.);
#1744=B_SPLINE_CURVE_WITH_KNOTS('',3,(#12505,#12506,#12507,#12508,#12509,
#12510,#12511,#12512,#12513,#12514),.UNSPECIFIED.,.F.,.F.,(4,2,2,2,4),(-0.147143178540475,
-0.1468201126579,-0.121744812771334,-0.102578136276002,-0.0907850237818083),
 .UNSPECIFIED.);
#1745=VERTEX_POINT('',#6235);
#1746=VERTEX_POINT('',#6236);
#1747=VERTEX_POINT('',#6284);
#1748=VERTEX_POINT('',#6286);
#1749=VERTEX_POINT('',#6357);
#1750=VERTEX_POINT('',#6646);
#1751=VERTEX_POINT('',#6697);
#1752=VERTEX_POINT('',#6701);
#1753=VERTEX_POINT('',#6787);
#1754=VERTEX_POINT('',#7076);
#1755=VERTEX_POINT('',#7202);
#1756=VERTEX_POINT('',#7224);
#1757=VERTEX_POINT('',#7225);
#1758=VERTEX_POINT('',#7304);
#1759=VERTEX_POINT('',#7356);
#1760=VERTEX_POINT('',#7359);
#1761=VERTEX_POINT('',#7360);
#1762=VERTEX_POINT('',#7362);
#1763=VERTEX_POINT('',#7364);
#1764=VERTEX_POINT('',#7366);
#1765=VERTEX_POINT('',#7407);
#1766=VERTEX_POINT('',#7408);
#1767=VERTEX_POINT('',#7421);
#1768=VERTEX_POINT('',#7422);
#1769=VERTEX_POINT('',#7451);
#1770=VERTEX_POINT('',#7452);
#1771=VERTEX_POINT('',#7465);
#1772=VERTEX_POINT('',#7483);
#1773=VERTEX_POINT('',#7490);
#1774=VERTEX_POINT('',#7505);
#1775=VERTEX_POINT('',#7507);
#1776=VERTEX_POINT('',#7535);
#1777=VERTEX_POINT('',#7536);
#1778=VERTEX_POINT('',#7549);
#1779=VERTEX_POINT('',#7550);
#1780=VERTEX_POINT('',#7579);
#1781=VERTEX_POINT('',#7580);
#1782=VERTEX_POINT('',#7593);
#1783=VERTEX_POINT('',#7594);
#1784=VERTEX_POINT('',#7610);
#1785=VERTEX_POINT('',#7614);
#1786=VERTEX_POINT('',#7633);
#1787=VERTEX_POINT('',#7635);
#1788=VERTEX_POINT('',#7637);
#1789=VERTEX_POINT('',#7646);
#1790=VERTEX_POINT('',#7648);
#1791=VERTEX_POINT('',#7650);
#1792=VERTEX_POINT('',#7654);
#1793=VERTEX_POINT('',#7656);
#1794=VERTEX_POINT('',#7660);
#1795=VERTEX_POINT('',#7663);
#1796=VERTEX_POINT('',#7665);
#1797=VERTEX_POINT('',#7669);
#1798=VERTEX_POINT('',#7671);
#1799=VERTEX_POINT('',#7675);
#1800=VERTEX_POINT('',#7677);
#1801=VERTEX_POINT('',#7681);
#1802=VERTEX_POINT('',#7683);
#1803=VERTEX_POINT('',#7687);
#1804=VERTEX_POINT('',#7689);
#1805=VERTEX_POINT('',#7693);
#1806=VERTEX_POINT('',#7695);
#1807=VERTEX_POINT('',#7699);
#1808=VERTEX_POINT('',#7701);
#1809=VERTEX_POINT('',#7705);
#1810=VERTEX_POINT('',#7707);
#1811=VERTEX_POINT('',#7711);
#1812=VERTEX_POINT('',#7715);
#1813=VERTEX_POINT('',#7718);
#1814=VERTEX_POINT('',#7720);
#1815=VERTEX_POINT('',#7724);
#1816=VERTEX_POINT('',#7725);
#1817=VERTEX_POINT('',#7733);
#1818=VERTEX_POINT('',#7734);
#1819=VERTEX_POINT('',#7736);
#1820=VERTEX_POINT('',#7750);
#1821=VERTEX_POINT('',#7775);
#1822=VERTEX_POINT('',#7776);
#1823=VERTEX_POINT('',#7823);
#1824=VERTEX_POINT('',#7824);
#1825=VERTEX_POINT('',#7874);
#1826=VERTEX_POINT('',#7875);
#1827=VERTEX_POINT('',#7925);
#1828=VERTEX_POINT('',#7926);
#1829=VERTEX_POINT('',#7973);
#1830=VERTEX_POINT('',#7974);
#1831=VERTEX_POINT('',#8024);
#1832=VERTEX_POINT('',#8025);
#1833=VERTEX_POINT('',#8072);
#1834=VERTEX_POINT('',#8073);
#1835=VERTEX_POINT('',#8123);
#1836=VERTEX_POINT('',#8124);
#1837=VERTEX_POINT('',#8174);
#1838=VERTEX_POINT('',#8175);
#1839=VERTEX_POINT('',#8222);
#1840=VERTEX_POINT('',#8223);
#1841=VERTEX_POINT('',#8273);
#1842=VERTEX_POINT('',#8274);
#1843=VERTEX_POINT('',#8324);
#1844=VERTEX_POINT('',#8325);
#1845=VERTEX_POINT('',#8372);
#1846=VERTEX_POINT('',#8373);
#1847=VERTEX_POINT('',#8423);
#1848=VERTEX_POINT('',#8424);
#1849=VERTEX_POINT('',#8471);
#1850=VERTEX_POINT('',#8472);
#1851=VERTEX_POINT('',#8522);
#1852=VERTEX_POINT('',#8523);
#1853=VERTEX_POINT('',#8525);
#1854=VERTEX_POINT('',#8539);
#1855=VERTEX_POINT('',#8564);
#1856=VERTEX_POINT('',#8565);
#1857=VERTEX_POINT('',#8567);
#1858=VERTEX_POINT('',#8572);
#1859=VERTEX_POINT('',#8581);
#1860=VERTEX_POINT('',#8582);
#1861=VERTEX_POINT('',#8606);
#1862=VERTEX_POINT('',#8607);
#1863=VERTEX_POINT('',#8631);
#1864=VERTEX_POINT('',#8632);
#1865=VERTEX_POINT('',#8655);
#1866=VERTEX_POINT('',#8656);
#1867=VERTEX_POINT('',#8680);
#1868=VERTEX_POINT('',#8681);
#1869=VERTEX_POINT('',#8705);
#1870=VERTEX_POINT('',#8706);
#1871=VERTEX_POINT('',#8729);
#1872=VERTEX_POINT('',#8730);
#1873=VERTEX_POINT('',#8753);
#1874=VERTEX_POINT('',#8754);
#1875=VERTEX_POINT('',#8779);
#1876=VERTEX_POINT('',#8780);
#1877=VERTEX_POINT('',#8803);
#1878=VERTEX_POINT('',#8804);
#1879=VERTEX_POINT('',#8827);
#1880=VERTEX_POINT('',#8828);
#1881=VERTEX_POINT('',#8853);
#1882=VERTEX_POINT('',#8854);
#1883=VERTEX_POINT('',#8877);
#1884=VERTEX_POINT('',#8878);
#1885=VERTEX_POINT('',#8901);
#1886=VERTEX_POINT('',#8902);
#1887=VERTEX_POINT('',#8926);
#1888=VERTEX_POINT('',#8927);
#1889=VERTEX_POINT('',#8951);
#1890=VERTEX_POINT('',#8952);
#1891=VERTEX_POINT('',#8975);
#1892=VERTEX_POINT('',#8976);
#1893=VERTEX_POINT('',#8978);
#1894=VERTEX_POINT('',#8984);
#1895=VERTEX_POINT('',#8993);
#1896=VERTEX_POINT('',#9832);
#1897=VERTEX_POINT('',#10318);
#1898=VERTEX_POINT('',#10322);
#1899=VERTEX_POINT('',#10326);
#1900=VERTEX_POINT('',#10327);
#1901=VERTEX_POINT('',#10329);
#1902=VERTEX_POINT('',#10331);
#1903=VERTEX_POINT('',#10335);
#1904=VERTEX_POINT('',#10337);
#1905=VERTEX_POINT('',#10341);
#1906=VERTEX_POINT('',#10343);
#1907=VERTEX_POINT('',#10351);
#1908=VERTEX_POINT('',#10352);
#1909=VERTEX_POINT('',#10354);
#1910=VERTEX_POINT('',#10356);
#1911=VERTEX_POINT('',#10360);
#1912=VERTEX_POINT('',#10362);
#1913=VERTEX_POINT('',#10366);
#1914=VERTEX_POINT('',#10368);
#1915=VERTEX_POINT('',#10376);
#1916=VERTEX_POINT('',#10378);
#1917=VERTEX_POINT('',#10381);
#1918=VERTEX_POINT('',#10385);
#1919=VERTEX_POINT('',#10388);
#1920=VERTEX_POINT('',#10392);
#1921=VERTEX_POINT('',#10395);
#1922=VERTEX_POINT('',#10399);
#1923=VERTEX_POINT('',#10402);
#1924=VERTEX_POINT('',#10406);
#1925=VERTEX_POINT('',#10411);
#1926=VERTEX_POINT('',#10415);
#1927=VERTEX_POINT('',#10421);
#1928=VERTEX_POINT('',#10422);
#1929=VERTEX_POINT('',#10424);
#1930=VERTEX_POINT('',#10426);
#1931=VERTEX_POINT('',#10430);
#1932=VERTEX_POINT('',#10438);
#1933=VERTEX_POINT('',#10465);
#1934=VERTEX_POINT('',#10470);
#1935=VERTEX_POINT('',#10477);
#1936=VERTEX_POINT('',#10479);
#1937=VERTEX_POINT('',#10483);
#1938=VERTEX_POINT('',#10594);
#1939=VERTEX_POINT('',#10595);
#1940=VERTEX_POINT('',#10619);
#1941=VERTEX_POINT('',#10644);
#1942=VERTEX_POINT('',#10693);
#1943=VERTEX_POINT('',#10698);
#1944=VERTEX_POINT('',#10724);
#1945=VERTEX_POINT('',#10915);
#1946=VERTEX_POINT('',#10920);
#1947=VERTEX_POINT('',#10925);
#1948=VERTEX_POINT('',#10984);
#1949=VERTEX_POINT('',#10989);
#1950=VERTEX_POINT('',#11007);
#1951=VERTEX_POINT('',#11105);
#1952=VERTEX_POINT('',#11107);
#1953=VERTEX_POINT('',#11136);
#1954=VERTEX_POINT('',#11140);
#1955=VERTEX_POINT('',#11141);
#1956=VERTEX_POINT('',#11144);
#1957=VERTEX_POINT('',#11148);
#1958=VERTEX_POINT('',#11149);
#1959=VERTEX_POINT('',#11151);
#1960=VERTEX_POINT('',#11153);
#1961=VERTEX_POINT('',#11157);
#1962=VERTEX_POINT('',#11161);
#1963=VERTEX_POINT('',#11163);
#1964=VERTEX_POINT('',#11167);
#1965=VERTEX_POINT('',#11171);
#1966=VERTEX_POINT('',#11175);
#1967=VERTEX_POINT('',#11179);
#1968=VERTEX_POINT('',#11181);
#1969=VERTEX_POINT('',#11185);
#1970=VERTEX_POINT('',#11189);
#1971=VERTEX_POINT('',#11193);
#1972=VERTEX_POINT('',#11195);
#1973=VERTEX_POINT('',#11199);
#1974=VERTEX_POINT('',#11205);
#1975=VERTEX_POINT('',#11207);
#1976=VERTEX_POINT('',#11211);
#1977=VERTEX_POINT('',#11213);
#1978=VERTEX_POINT('',#11215);
#1979=VERTEX_POINT('',#11221);
#1980=VERTEX_POINT('',#11223);
#1981=VERTEX_POINT('',#11227);
#1982=VERTEX_POINT('',#11233);
#1983=VERTEX_POINT('',#11348);
#1984=VERTEX_POINT('',#11350);
#1985=VERTEX_POINT('',#11374);
#1986=VERTEX_POINT('',#11397);
#1987=VERTEX_POINT('',#11402);
#1988=VERTEX_POINT('',#11646);
#1989=VERTEX_POINT('',#11651);
#1990=VERTEX_POINT('',#11695);
#1991=VERTEX_POINT('',#11700);
#1992=VERTEX_POINT('',#11737);
#1993=VERTEX_POINT('',#11742);
#1994=VERTEX_POINT('',#11752);
#1995=VERTEX_POINT('',#11757);
#1996=VERTEX_POINT('',#11790);
#1997=VERTEX_POINT('',#11791);
#1998=VERTEX_POINT('',#11794);
#1999=VERTEX_POINT('',#11798);
#2000=VERTEX_POINT('',#11799);
#2001=VERTEX_POINT('',#11804);
#2002=VERTEX_POINT('',#11807);
#2003=VERTEX_POINT('',#11811);
#2004=VERTEX_POINT('',#11814);
#2005=VERTEX_POINT('',#11815);
#2006=VERTEX_POINT('',#11817);
#2007=VERTEX_POINT('',#11819);
#2008=VERTEX_POINT('',#11823);
#2009=VERTEX_POINT('',#11824);
#2010=VERTEX_POINT('',#11826);
#2011=VERTEX_POINT('',#11828);
#2012=VERTEX_POINT('',#11832);
#2013=VERTEX_POINT('',#11836);
#2014=VERTEX_POINT('',#11840);
#2015=VERTEX_POINT('',#11844);
#2016=VERTEX_POINT('',#11848);
#2017=VERTEX_POINT('',#11850);
#2018=VERTEX_POINT('',#11852);
#2019=VERTEX_POINT('',#11857);
#2020=VERTEX_POINT('',#11859);
#2021=VERTEX_POINT('',#11861);
#2022=VERTEX_POINT('',#11866);
#2023=VERTEX_POINT('',#11895);
#2024=VERTEX_POINT('',#11900);
#2025=VERTEX_POINT('',#11902);
#2026=VERTEX_POINT('',#12038);
#2027=VERTEX_POINT('',#12039);
#2028=VERTEX_POINT('',#12131);
#2029=VERTEX_POINT('',#12132);
#2030=VERTEX_POINT('',#12135);
#2031=VERTEX_POINT('',#12137);
#2032=VERTEX_POINT('',#12143);
#2033=VERTEX_POINT('',#12144);
#2034=VERTEX_POINT('',#12149);
#2035=VERTEX_POINT('',#12151);
#2036=VERTEX_POINT('',#12155);
#2037=VERTEX_POINT('',#12157);
#2038=VERTEX_POINT('',#12162);
#2039=VERTEX_POINT('',#12167);
#2040=VERTEX_POINT('',#12172);
#2041=VERTEX_POINT('',#12198);
#2042=VERTEX_POINT('',#12200);
#2043=VERTEX_POINT('',#12231);
#2044=VERTEX_POINT('',#12236);
#2045=VERTEX_POINT('',#12335);
#2046=VERTEX_POINT('',#12419);
#2047=VERTEX_POINT('',#12426);
#2048=VERTEX_POINT('',#12428);
#2049=VERTEX_POINT('',#12437);
#2050=VERTEX_POINT('',#12439);
#2051=VERTEX_POINT('',#12441);
#2052=VERTEX_POINT('',#12446);
#2053=VERTEX_POINT('',#12450);
#2054=VERTEX_POINT('',#12454);
#2055=VERTEX_POINT('',#12460);
#2056=VERTEX_POINT('',#12464);
#2057=VERTEX_POINT('',#12467);
#2058=VERTEX_POINT('',#12468);
#2059=VERTEX_POINT('',#12473);
#2060=VERTEX_POINT('',#12475);
#2061=VERTEX_POINT('',#12477);
#2062=VERTEX_POINT('',#12479);
#2063=VERTEX_POINT('',#12481);
#2064=VERTEX_POINT('',#12520);
#2065=VERTEX_POINT('',#12522);
#2066=VERTEX_POINT('',#12524);
#2067=VERTEX_POINT('',#12528);
#2068=VERTEX_POINT('',#12530);
#2069=VERTEX_POINT('',#12534);
#2070=VERTEX_POINT('',#12537);
#2071=VERTEX_POINT('',#12539);
#2072=VERTEX_POINT('',#12543);
#2073=VERTEX_POINT('',#12545);
#2074=VERTEX_POINT('',#12549);
#2075=VERTEX_POINT('',#12553);
#2076=VERTEX_POINT('',#12556);
#2077=VERTEX_POINT('',#12558);
#2078=VERTEX_POINT('',#12562);
#2079=VERTEX_POINT('',#12563);
#2080=VERTEX_POINT('',#12571);
#2081=VERTEX_POINT('',#12573);
#2082=VERTEX_POINT('',#12577);
#2083=VERTEX_POINT('',#12580);
#2084=VERTEX_POINT('',#12584);
#2085=VERTEX_POINT('',#12588);
#2086=VERTEX_POINT('',#12594);
#2087=VERTEX_POINT('',#12596);
#2088=VERTEX_POINT('',#12600);
#2089=VERTEX_POINT('',#12604);
#2090=VERTEX_POINT('',#12608);
#2091=VERTEX_POINT('',#12611);
#2092=VERTEX_POINT('',#12617);
#2093=VERTEX_POINT('',#12619);
#2094=VERTEX_POINT('',#12623);
#2095=VERTEX_POINT('',#12625);
#2096=VERTEX_POINT('',#12629);
#2097=VERTEX_POINT('',#12630);
#2098=VERTEX_POINT('',#12632);
#2099=VERTEX_POINT('',#12634);
#2100=VERTEX_POINT('',#12636);
#2101=VERTEX_POINT('',#12638);
#2102=VERTEX_POINT('',#12640);
#2103=VERTEX_POINT('',#12642);
#2104=VERTEX_POINT('',#12646);
#2105=VERTEX_POINT('',#12648);
#2106=VERTEX_POINT('',#12652);
#2107=VERTEX_POINT('',#12656);
#2108=VERTEX_POINT('',#12660);
#2109=VERTEX_POINT('',#12661);
#2110=VERTEX_POINT('',#12664);
#2111=VERTEX_POINT('',#12666);
#2112=VERTEX_POINT('',#12680);
#2113=VERTEX_POINT('',#12681);
#2114=VERTEX_POINT('',#12683);
#2115=VERTEX_POINT('',#12687);
#2116=VERTEX_POINT('',#12688);
#2117=VERTEX_POINT('',#12690);
#2118=VERTEX_POINT('',#12694);
#2119=VERTEX_POINT('',#12695);
#2120=VERTEX_POINT('',#12697);
#2121=VERTEX_POINT('',#12701);
#2122=VERTEX_POINT('',#12702);
#2123=VERTEX_POINT('',#12704);
#2124=VERTEX_POINT('',#12711);
#2125=VERTEX_POINT('',#12712);
#2126=VERTEX_POINT('',#12714);
#2127=VERTEX_POINT('',#12718);
#2128=VERTEX_POINT('',#12719);
#2129=VERTEX_POINT('',#12721);
#2130=VERTEX_POINT('',#12728);
#2131=VERTEX_POINT('',#12729);
#2132=VERTEX_POINT('',#12731);
#2133=VERTEX_POINT('',#12741);
#2134=VERTEX_POINT('',#12742);
#2135=VERTEX_POINT('',#12744);
#2136=EDGE_CURVE('',#1745,#1746,#1583,.T.);
#2137=EDGE_CURVE('',#1746,#1745,#1584,.T.);
#2138=EDGE_CURVE('',#1746,#1747,#1123,.T.);
#2139=EDGE_CURVE('',#1748,#1747,#892,.T.);
#2140=EDGE_CURVE('',#1747,#1748,#893,.T.);
#2141=EDGE_CURVE('',#1749,#1745,#894,.T.);
#2142=EDGE_CURVE('',#1749,#1749,#1585,.T.);
#2143=EDGE_CURVE('',#1750,#1749,#290,.T.);
#2144=EDGE_CURVE('',#1750,#1750,#1586,.T.);
#2145=EDGE_CURVE('',#1748,#1751,#895,.T.);
#2146=EDGE_CURVE('',#1751,#1751,#896,.T.);
#2147=EDGE_CURVE('',#1752,#1752,#1587,.T.);
#2148=EDGE_CURVE('',#1752,#1753,#897,.T.);
#2149=EDGE_CURVE('',#1753,#1753,#1588,.T.);
#2150=EDGE_CURVE('',#1753,#1754,#291,.T.);
#2151=EDGE_CURVE('',#1754,#1754,#1589,.T.);
#2152=EDGE_CURVE('',#1754,#1755,#898,.T.);
#2153=EDGE_CURVE('',#1755,#1755,#1590,.T.);
#2154=EDGE_CURVE('',#1756,#1757,#899,.T.);
#2155=EDGE_CURVE('',#1757,#1756,#900,.T.);
#2156=EDGE_CURVE('',#1758,#1750,#901,.T.);
#2157=EDGE_CURVE('',#1758,#1758,#1591,.T.);
#2158=EDGE_CURVE('',#1759,#1759,#902,.T.);
#2159=EDGE_CURVE('',#1760,#1761,#903,.F.);
#2160=EDGE_CURVE('',#1761,#1762,#1124,.T.);
#2161=EDGE_CURVE('',#1762,#1763,#904,.T.);
#2162=EDGE_CURVE('',#1763,#1764,#1125,.T.);
#2163=EDGE_CURVE('',#1764,#1760,#1592,.F.);
#2164=EDGE_CURVE('',#1765,#1766,#905,.T.);
#2165=EDGE_CURVE('',#1766,#1763,#1593,.T.);
#2166=EDGE_CURVE('',#1762,#1765,#1594,.T.);
#2167=EDGE_CURVE('',#1767,#1768,#906,.T.);
#2168=EDGE_CURVE('',#1768,#1766,#1126,.T.);
#2169=EDGE_CURVE('',#1765,#1767,#1127,.T.);
#2170=EDGE_CURVE('',#1769,#1770,#907,.T.);
#2171=EDGE_CURVE('',#1770,#1768,#1595,.T.);
#2172=EDGE_CURVE('',#1767,#1769,#1596,.T.);
#2173=EDGE_CURVE('',#1756,#1771,#1597,.T.);
#2174=EDGE_CURVE('',#1756,#1770,#1128,.T.);
#2175=EDGE_CURVE('',#1769,#1771,#1129,.T.);
#2176=EDGE_CURVE('',#1772,#1761,#1130,.T.);
#2177=EDGE_CURVE('',#1771,#1772,#1598,.F.);
#2178=EDGE_CURVE('',#1757,#1773,#1599,.F.);
#2179=EDGE_CURVE('',#1773,#1774,#1131,.T.);
#2180=EDGE_CURVE('',#1774,#1775,#908,.T.);
#2181=EDGE_CURVE('',#1775,#1757,#1132,.T.);
#2182=EDGE_CURVE('',#1776,#1777,#909,.T.);
#2183=EDGE_CURVE('',#1777,#1775,#1600,.T.);
#2184=EDGE_CURVE('',#1774,#1776,#1601,.T.);
#2185=EDGE_CURVE('',#1778,#1779,#910,.T.);
#2186=EDGE_CURVE('',#1779,#1777,#1133,.T.);
#2187=EDGE_CURVE('',#1776,#1778,#1134,.T.);
#2188=EDGE_CURVE('',#1780,#1781,#911,.T.);
#2189=EDGE_CURVE('',#1781,#1779,#1602,.T.);
#2190=EDGE_CURVE('',#1778,#1780,#1603,.T.);
#2191=EDGE_CURVE('',#1782,#1783,#1604,.T.);
#2192=EDGE_CURVE('',#1782,#1781,#1135,.T.);
#2193=EDGE_CURVE('',#1780,#1784,#1136,.T.);
#2194=EDGE_CURVE('',#1783,#1784,#912,.T.);
#2195=EDGE_CURVE('',#1785,#1773,#1605,.F.);
#2196=EDGE_CURVE('',#1784,#1785,#1137,.T.);
#2197=EDGE_CURVE('',#1783,#1760,#913,.F.);
#2198=EDGE_CURVE('',#1764,#1782,#914,.T.);
#2199=EDGE_CURVE('',#1772,#1785,#915,.T.);
#2200=EDGE_CURVE('',#1770,#1775,#916,.T.);
#2201=EDGE_CURVE('',#1777,#1768,#917,.T.);
#2202=EDGE_CURVE('',#1766,#1779,#918,.T.);
#2203=EDGE_CURVE('',#1786,#1763,#919,.T.);
#2204=EDGE_CURVE('',#1786,#1787,#1138,.T.);
#2205=EDGE_CURVE('',#1788,#1787,#920,.T.);
#2206=EDGE_CURVE('',#1787,#1788,#921,.T.);
#2207=EDGE_CURVE('',#1781,#1786,#922,.T.);
#2208=EDGE_CURVE('',#1788,#1759,#923,.T.);
#2209=EDGE_CURVE('',#1789,#1789,#924,.T.);
#2210=EDGE_CURVE('',#1789,#1790,#925,.T.);
#2211=EDGE_CURVE('',#1790,#1791,#926,.T.);
#2212=EDGE_CURVE('',#1791,#1790,#927,.T.);
#2213=EDGE_CURVE('',#1791,#1792,#1139,.T.);
#2214=EDGE_CURVE('',#1793,#1792,#928,.T.);
#2215=EDGE_CURVE('',#1792,#1793,#929,.T.);
#2216=EDGE_CURVE('',#1794,#1794,#930,.T.);
#2217=EDGE_CURVE('',#1793,#1795,#931,.T.);
#2218=EDGE_CURVE('',#1795,#1796,#932,.T.);
#2219=EDGE_CURVE('',#1796,#1795,#933,.T.);
#2220=EDGE_CURVE('',#1796,#1797,#1140,.T.);
#2221=EDGE_CURVE('',#1798,#1797,#934,.T.);
#2222=EDGE_CURVE('',#1797,#1798,#935,.T.);
#2223=EDGE_CURVE('',#1798,#1799,#936,.T.);
#2224=EDGE_CURVE('',#1799,#1800,#937,.T.);
#2225=EDGE_CURVE('',#1800,#1799,#938,.T.);
#2226=EDGE_CURVE('',#1800,#1801,#1141,.T.);
#2227=EDGE_CURVE('',#1802,#1801,#939,.T.);
#2228=EDGE_CURVE('',#1801,#1802,#940,.T.);
#2229=EDGE_CURVE('',#1802,#1803,#941,.T.);
#2230=EDGE_CURVE('',#1803,#1804,#942,.T.);
#2231=EDGE_CURVE('',#1804,#1803,#943,.T.);
#2232=EDGE_CURVE('',#1804,#1805,#1142,.T.);
#2233=EDGE_CURVE('',#1806,#1805,#944,.T.);
#2234=EDGE_CURVE('',#1805,#1806,#945,.T.);
#2235=EDGE_CURVE('',#1806,#1807,#946,.T.);
#2236=EDGE_CURVE('',#1807,#1808,#947,.T.);
#2237=EDGE_CURVE('',#1808,#1807,#948,.T.);
#2238=EDGE_CURVE('',#1808,#1809,#1143,.T.);
#2239=EDGE_CURVE('',#1810,#1809,#949,.T.);
#2240=EDGE_CURVE('',#1809,#1810,#950,.T.);
#2241=EDGE_CURVE('',#1810,#1811,#951,.T.);
#2242=EDGE_CURVE('',#1811,#1811,#952,.T.);
#2243=EDGE_CURVE('',#1812,#1812,#953,.T.);
#2244=EDGE_CURVE('',#1812,#1813,#954,.T.);
#2245=EDGE_CURVE('',#1813,#1814,#955,.T.);
#2246=EDGE_CURVE('',#1814,#1813,#956,.T.);
#2247=EDGE_CURVE('',#1815,#1816,#957,.T.);
#2248=EDGE_CURVE('',#1816,#1815,#958,.T.);
#2249=EDGE_CURVE('',#1816,#1814,#1144,.T.);
#2250=EDGE_CURVE('',#1815,#1794,#959,.T.);
#2251=EDGE_CURVE('',#1817,#1818,#1145,.T.);
#2252=EDGE_CURVE('',#1818,#1819,#1606,.T.);
#2253=EDGE_CURVE('',#1819,#1820,#960,.T.);
#2254=EDGE_CURVE('',#1820,#1817,#1607,.T.);
#2255=EDGE_CURVE('',#1821,#1822,#1146,.T.);
#2256=EDGE_CURVE('',#1822,#1818,#1608,.T.);
#2257=EDGE_CURVE('',#1817,#1821,#1609,.T.);
#2258=EDGE_CURVE('',#1823,#1824,#1147,.T.);
#2259=EDGE_CURVE('',#1824,#1822,#1610,.T.);
#2260=EDGE_CURVE('',#1821,#1823,#1611,.T.);
#2261=EDGE_CURVE('',#1825,#1826,#1148,.T.);
#2262=EDGE_CURVE('',#1826,#1824,#1612,.T.);
#2263=EDGE_CURVE('',#1823,#1825,#1613,.T.);
#2264=EDGE_CURVE('',#1827,#1828,#1149,.T.);
#2265=EDGE_CURVE('',#1828,#1826,#1614,.T.);
#2266=EDGE_CURVE('',#1825,#1827,#1615,.T.);
#2267=EDGE_CURVE('',#1829,#1830,#1150,.T.);
#2268=EDGE_CURVE('',#1830,#1828,#1616,.T.);
#2269=EDGE_CURVE('',#1827,#1829,#1617,.T.);
#2270=EDGE_CURVE('',#1831,#1832,#1151,.T.);
#2271=EDGE_CURVE('',#1832,#1830,#1618,.T.);
#2272=EDGE_CURVE('',#1829,#1831,#1619,.T.);
#2273=EDGE_CURVE('',#1833,#1834,#1152,.T.);
#2274=EDGE_CURVE('',#1834,#1832,#1620,.T.);
#2275=EDGE_CURVE('',#1831,#1833,#1621,.T.);
#2276=EDGE_CURVE('',#1835,#1836,#1153,.T.);
#2277=EDGE_CURVE('',#1836,#1834,#1622,.T.);
#2278=EDGE_CURVE('',#1833,#1835,#1623,.T.);
#2279=EDGE_CURVE('',#1837,#1838,#1154,.T.);
#2280=EDGE_CURVE('',#1838,#1836,#1624,.T.);
#2281=EDGE_CURVE('',#1835,#1837,#1625,.T.);
#2282=EDGE_CURVE('',#1839,#1840,#1155,.T.);
#2283=EDGE_CURVE('',#1840,#1838,#1626,.T.);
#2284=EDGE_CURVE('',#1837,#1839,#1627,.T.);
#2285=EDGE_CURVE('',#1841,#1842,#1156,.T.);
#2286=EDGE_CURVE('',#1842,#1840,#1628,.T.);
#2287=EDGE_CURVE('',#1839,#1841,#1629,.T.);
#2288=EDGE_CURVE('',#1843,#1844,#1157,.T.);
#2289=EDGE_CURVE('',#1844,#1842,#1630,.T.);
#2290=EDGE_CURVE('',#1841,#1843,#1631,.T.);
#2291=EDGE_CURVE('',#1845,#1846,#1158,.T.);
#2292=EDGE_CURVE('',#1846,#1844,#1632,.T.);
#2293=EDGE_CURVE('',#1843,#1845,#1633,.T.);
#2294=EDGE_CURVE('',#1847,#1848,#1159,.T.);
#2295=EDGE_CURVE('',#1848,#1846,#1634,.T.);
#2296=EDGE_CURVE('',#1845,#1847,#1635,.T.);
#2297=EDGE_CURVE('',#1849,#1850,#1160,.T.);
#2298=EDGE_CURVE('',#1850,#1848,#1636,.T.);
#2299=EDGE_CURVE('',#1847,#1849,#1637,.T.);
#2300=EDGE_CURVE('',#1851,#1852,#1161,.T.);
#2301=EDGE_CURVE('',#1851,#1853,#1638,.T.);
#2302=EDGE_CURVE('',#1854,#1853,#961,.T.);
#2303=EDGE_CURVE('',#1854,#1852,#1639,.T.);
#2304=EDGE_CURVE('',#1855,#1856,#1162,.T.);
#2305=EDGE_CURVE('',#1856,#1857,#1640,.T.);
#2306=EDGE_CURVE('',#1858,#1857,#962,.T.);
#2307=EDGE_CURVE('',#1855,#1858,#1641,.T.);
#2308=EDGE_CURVE('',#1859,#1860,#1163,.T.);
#2309=EDGE_CURVE('',#1860,#1856,#1642,.T.);
#2310=EDGE_CURVE('',#1859,#1855,#1643,.T.);
#2311=EDGE_CURVE('',#1861,#1862,#1164,.T.);
#2312=EDGE_CURVE('',#1862,#1860,#1644,.T.);
#2313=EDGE_CURVE('',#1861,#1859,#1645,.T.);
#2314=EDGE_CURVE('',#1863,#1864,#1165,.T.);
#2315=EDGE_CURVE('',#1864,#1862,#1646,.T.);
#2316=EDGE_CURVE('',#1863,#1861,#1647,.T.);
#2317=EDGE_CURVE('',#1865,#1866,#1166,.T.);
#2318=EDGE_CURVE('',#1866,#1864,#1648,.T.);
#2319=EDGE_CURVE('',#1865,#1863,#1649,.T.);
#2320=EDGE_CURVE('',#1867,#1868,#1167,.T.);
#2321=EDGE_CURVE('',#1868,#1866,#1650,.T.);
#2322=EDGE_CURVE('',#1867,#1865,#1651,.T.);
#2323=EDGE_CURVE('',#1869,#1870,#1168,.T.);
#2324=EDGE_CURVE('',#1870,#1868,#1652,.T.);
#2325=EDGE_CURVE('',#1869,#1867,#1653,.T.);
#2326=EDGE_CURVE('',#1871,#1872,#1169,.T.);
#2327=EDGE_CURVE('',#1872,#1870,#1654,.T.);
#2328=EDGE_CURVE('',#1871,#1869,#1655,.T.);
#2329=EDGE_CURVE('',#1873,#1874,#1170,.T.);
#2330=EDGE_CURVE('',#1874,#1872,#1656,.T.);
#2331=EDGE_CURVE('',#1873,#1871,#1657,.T.);
#2332=EDGE_CURVE('',#1875,#1876,#1171,.T.);
#2333=EDGE_CURVE('',#1876,#1874,#1658,.T.);
#2334=EDGE_CURVE('',#1875,#1873,#1659,.T.);
#2335=EDGE_CURVE('',#1877,#1878,#1172,.T.);
#2336=EDGE_CURVE('',#1878,#1876,#1660,.T.);
#2337=EDGE_CURVE('',#1877,#1875,#1661,.T.);
#2338=EDGE_CURVE('',#1879,#1880,#1173,.T.);
#2339=EDGE_CURVE('',#1880,#1878,#1662,.T.);
#2340=EDGE_CURVE('',#1879,#1877,#1663,.T.);
#2341=EDGE_CURVE('',#1881,#1882,#1174,.T.);
#2342=EDGE_CURVE('',#1882,#1880,#1664,.T.);
#2343=EDGE_CURVE('',#1881,#1879,#1665,.T.);
#2344=EDGE_CURVE('',#1883,#1884,#1175,.T.);
#2345=EDGE_CURVE('',#1884,#1882,#1666,.T.);
#2346=EDGE_CURVE('',#1883,#1881,#1667,.T.);
#2347=EDGE_CURVE('',#1885,#1886,#1176,.T.);
#2348=EDGE_CURVE('',#1886,#1884,#1668,.T.);
#2349=EDGE_CURVE('',#1885,#1883,#1669,.T.);
#2350=EDGE_CURVE('',#1887,#1888,#1177,.T.);
#2351=EDGE_CURVE('',#1888,#1886,#1670,.T.);
#2352=EDGE_CURVE('',#1887,#1885,#1671,.T.);
#2353=EDGE_CURVE('',#1889,#1890,#1178,.T.);
#2354=EDGE_CURVE('',#1890,#1888,#1672,.T.);
#2355=EDGE_CURVE('',#1889,#1887,#1673,.T.);
#2356=EDGE_CURVE('',#1891,#1892,#1179,.T.);
#2357=EDGE_CURVE('',#1893,#1891,#1674,.T.);
#2358=EDGE_CURVE('',#1894,#1893,#963,.T.);
#2359=EDGE_CURVE('',#1894,#1892,#1675,.T.);
#2360=EDGE_CURVE('',#1820,#1895,#964,.T.);
#2361=EDGE_CURVE('',#1895,#1819,#965,.T.);
#2362=EDGE_CURVE('',#1819,#1858,#1676,.T.);
#2363=EDGE_CURVE('',#1857,#1820,#1677,.T.);
#2364=EDGE_CURVE('',#1892,#1890,#1678,.T.);
#2365=EDGE_CURVE('',#1891,#1889,#1679,.T.);
#2366=EDGE_CURVE('',#1853,#1894,#1680,.T.);
#2367=EDGE_CURVE('',#1849,#1851,#1681,.T.);
#2368=EDGE_CURVE('',#1893,#1854,#1682,.T.);
#2369=EDGE_CURVE('',#1896,#1854,#966,.T.);
#2370=EDGE_CURVE('',#1853,#1896,#967,.T.);
#2371=EDGE_CURVE('',#1852,#1850,#1683,.T.);
#2372=EDGE_CURVE('',#1897,#1896,#1180,.T.);
#2373=EDGE_CURVE('',#1895,#1898,#1181,.T.);
#2374=EDGE_CURVE('',#1898,#1898,#968,.T.);
#2375=EDGE_CURVE('',#1899,#1900,#1182,.T.);
#2376=EDGE_CURVE('',#1901,#1899,#1183,.T.);
#2377=EDGE_CURVE('',#1902,#1901,#1184,.T.);
#2378=EDGE_CURVE('',#1900,#1902,#1185,.T.);
#2379=EDGE_CURVE('',#1900,#1903,#969,.T.);
#2380=EDGE_CURVE('',#1904,#1902,#1186,.T.);
#2381=EDGE_CURVE('',#1904,#1903,#1187,.T.);
#2382=EDGE_CURVE('',#1903,#1905,#1188,.T.);
#2383=EDGE_CURVE('',#1906,#1904,#1189,.T.);
#2384=EDGE_CURVE('',#1905,#1906,#1190,.T.);
#2385=EDGE_CURVE('',#1905,#1899,#970,.T.);
#2386=EDGE_CURVE('',#1906,#1901,#1191,.T.);
#2387=EDGE_CURVE('',#1907,#1908,#1192,.T.);
#2388=EDGE_CURVE('',#1909,#1907,#1193,.T.);
#2389=EDGE_CURVE('',#1910,#1909,#1194,.T.);
#2390=EDGE_CURVE('',#1908,#1910,#1195,.T.);
#2391=EDGE_CURVE('',#1908,#1911,#971,.T.);
#2392=EDGE_CURVE('',#1912,#1910,#1196,.T.);
#2393=EDGE_CURVE('',#1912,#1911,#1197,.T.);
#2394=EDGE_CURVE('',#1911,#1913,#1198,.T.);
#2395=EDGE_CURVE('',#1914,#1912,#1199,.T.);
#2396=EDGE_CURVE('',#1913,#1914,#1200,.T.);
#2397=EDGE_CURVE('',#1913,#1907,#972,.T.);
#2398=EDGE_CURVE('',#1914,#1909,#1201,.T.);
#2399=EDGE_CURVE('',#1915,#1915,#973,.T.);
#2400=EDGE_CURVE('',#1916,#1916,#974,.T.);
#2401=EDGE_CURVE('',#1917,#1917,#975,.T.);
#2402=EDGE_CURVE('',#1917,#1916,#1202,.T.);
#2403=EDGE_CURVE('',#1918,#1918,#976,.T.);
#2404=EDGE_CURVE('',#1918,#1919,#1203,.T.);
#2405=EDGE_CURVE('',#1919,#1919,#977,.T.);
#2406=EDGE_CURVE('',#1920,#1920,#978,.T.);
#2407=EDGE_CURVE('',#1921,#1921,#979,.T.);
#2408=EDGE_CURVE('',#1921,#1920,#1204,.T.);
#2409=EDGE_CURVE('',#1922,#1922,#980,.T.);
#2410=EDGE_CURVE('',#1922,#1923,#1205,.T.);
#2411=EDGE_CURVE('',#1923,#1923,#981,.T.);
#2412=EDGE_CURVE('',#1924,#1924,#982,.T.);
#2413=EDGE_CURVE('',#1923,#1924,#1206,.T.);
#2414=EDGE_CURVE('',#1925,#1925,#983,.T.);
#2415=EDGE_CURVE('',#1925,#1915,#1207,.T.);
#2416=EDGE_CURVE('',#1926,#1926,#984,.T.);
#2417=EDGE_CURVE('',#1926,#1925,#1208,.T.);
#2418=EDGE_CURVE('',#1927,#1928,#985,.T.);
#2419=EDGE_CURVE('',#1928,#1929,#986,.T.);
#2420=EDGE_CURVE('',#1929,#1930,#987,.T.);
#2421=EDGE_CURVE('',#1930,#1927,#988,.T.);
#2422=EDGE_CURVE('',#1929,#1931,#1684,.T.);
#2423=EDGE_CURVE('',#1931,#1930,#989,.T.);
#2424=EDGE_CURVE('',#1932,#1928,#1685,.T.);
#2425=EDGE_CURVE('',#1927,#1932,#990,.T.);
#2426=EDGE_CURVE('',#1932,#1933,#1686,.T.);
#2427=EDGE_CURVE('',#1934,#1933,#991,.T.);
#2428=EDGE_CURVE('',#1934,#1928,#1687,.T.);
#2429=EDGE_CURVE('',#1927,#1935,#1209,.T.);
#2430=EDGE_CURVE('',#1935,#1936,#992,.T.);
#2431=EDGE_CURVE('',#1936,#1932,#1210,.T.);
#2432=EDGE_CURVE('',#1937,#1930,#1211,.T.);
#2433=EDGE_CURVE('',#1935,#1937,#1688,.T.);
#2434=EDGE_CURVE('',#1938,#1939,#993,.T.);
#2435=EDGE_CURVE('',#1939,#1934,#1689,.T.);
#2436=EDGE_CURVE('',#1934,#1940,#994,.T.);
#2437=EDGE_CURVE('',#1940,#1938,#1690,.T.);
#2438=EDGE_CURVE('',#1938,#1941,#995,.T.);
#2439=EDGE_CURVE('',#1941,#1939,#996,.T.);
#2440=EDGE_CURVE('',#1933,#1940,#997,.T.);
#2441=EDGE_CURVE('',#1929,#1939,#1691,.T.);
#2442=EDGE_CURVE('',#1941,#1931,#1692,.T.);
#2443=EDGE_CURVE('',#1938,#1942,#1693,.T.);
#2444=EDGE_CURVE('',#1942,#1943,#1694,.T.);
#2445=EDGE_CURVE('',#1943,#1944,#1695,.T.);
#2446=EDGE_CURVE('',#1944,#1941,#1696,.T.);
#2447=EDGE_CURVE('',#1945,#1940,#1697,.T.);
#2448=EDGE_CURVE('',#1946,#1945,#1698,.T.);
#2449=EDGE_CURVE('',#1947,#1946,#292,.T.);
#2450=EDGE_CURVE('',#1947,#1947,#1699,.T.);
#2451=EDGE_CURVE('',#1942,#1946,#1700,.T.);
#2452=EDGE_CURVE('',#1933,#1948,#1701,.T.);
#2453=EDGE_CURVE('',#1948,#1949,#1702,.T.);
#2454=EDGE_CURVE('',#1945,#1949,#1703,.T.);
#2455=EDGE_CURVE('',#1950,#1936,#1704,.T.);
#2456=EDGE_CURVE('',#1948,#1950,#1212,.T.);
#2457=EDGE_CURVE('',#1947,#1951,#998,.T.);
#2458=EDGE_CURVE('',#1951,#1952,#1705,.T.);
#2459=EDGE_CURVE('',#1952,#1951,#1706,.T.);
#2460=EDGE_CURVE('',#1953,#1953,#999,.T.);
#2461=EDGE_CURVE('',#1953,#1952,#1213,.T.);
#2462=EDGE_CURVE('',#1954,#1955,#1000,.T.);
#2463=EDGE_CURVE('',#1955,#1954,#1001,.T.);
#2464=EDGE_CURVE('',#1954,#1956,#1002,.T.);
#2465=EDGE_CURVE('',#1956,#1956,#1003,.T.);
#2466=EDGE_CURVE('',#1957,#1958,#1214,.T.);
#2467=EDGE_CURVE('',#1959,#1957,#1004,.T.);
#2468=EDGE_CURVE('',#1960,#1959,#1215,.T.);
#2469=EDGE_CURVE('',#1958,#1960,#1216,.T.);
#2470=EDGE_CURVE('',#1961,#1961,#1005,.T.);
#2471=EDGE_CURVE('',#1961,#1955,#1217,.T.);
#2472=EDGE_CURVE('',#1960,#1962,#63,.F.);
#2473=EDGE_CURVE('',#1962,#1963,#1218,.T.);
#2474=EDGE_CURVE('',#1963,#1958,#64,.T.);
#2475=EDGE_CURVE('',#1963,#1964,#1219,.T.);
#2476=EDGE_CURVE('',#1964,#1957,#1006,.T.);
#2477=EDGE_CURVE('',#1964,#1965,#1007,.T.);
#2478=EDGE_CURVE('',#1965,#1957,#1008,.T.);
#2479=EDGE_CURVE('',#1965,#1966,#1009,.T.);
#2480=EDGE_CURVE('',#1966,#1959,#1010,.F.);
#2481=EDGE_CURVE('',#1964,#1967,#1220,.T.);
#2482=EDGE_CURVE('',#1968,#1967,#1011,.T.);
#2483=EDGE_CURVE('',#1968,#1965,#1221,.T.);
#2484=EDGE_CURVE('',#1969,#1963,#1222,.T.);
#2485=EDGE_CURVE('',#1967,#1969,#1223,.T.);
#2486=EDGE_CURVE('',#1962,#1970,#1224,.T.);
#2487=EDGE_CURVE('',#1969,#1970,#1225,.T.);
#2488=EDGE_CURVE('',#1970,#1971,#65,.F.);
#2489=EDGE_CURVE('',#1971,#1972,#1226,.T.);
#2490=EDGE_CURVE('',#1972,#1969,#66,.T.);
#2491=EDGE_CURVE('',#1967,#1973,#1012,.T.);
#2492=EDGE_CURVE('',#1973,#1968,#1013,.T.);
#2493=EDGE_CURVE('',#1972,#1973,#1227,.T.);
#2494=EDGE_CURVE('',#1973,#1974,#1014,.T.);
#2495=EDGE_CURVE('',#1974,#1975,#1015,.T.);
#2496=EDGE_CURVE('',#1975,#1968,#1016,.T.);
#2497=EDGE_CURVE('',#1976,#1976,#1017,.T.);
#2498=EDGE_CURVE('',#1976,#1977,#1018,.T.);
#2499=EDGE_CURVE('',#1977,#1978,#1019,.T.);
#2500=EDGE_CURVE('',#1978,#1977,#1020,.T.);
#2501=EDGE_CURVE('',#1974,#1971,#1228,.T.);
#2502=EDGE_CURVE('',#1978,#1979,#1229,.T.);
#2503=EDGE_CURVE('',#1979,#1980,#1021,.T.);
#2504=EDGE_CURVE('',#1980,#1979,#1022,.T.);
#2505=EDGE_CURVE('',#1981,#1966,#1023,.F.);
#2506=EDGE_CURVE('',#1959,#1981,#1024,.F.);
#2507=EDGE_CURVE('',#1981,#1962,#1230,.T.);
#2508=EDGE_CURVE('',#1975,#1982,#1025,.T.);
#2509=EDGE_CURVE('',#1982,#1981,#1231,.T.);
#2510=EDGE_CURVE('',#1966,#1975,#1232,.T.);
#2511=EDGE_CURVE('',#1974,#1982,#1026,.T.);
#2512=EDGE_CURVE('',#1970,#1982,#1233,.T.);
#2513=EDGE_CURVE('',#1937,#1983,#1027,.T.);
#2514=EDGE_CURVE('',#1983,#1984,#1707,.T.);
#2515=EDGE_CURVE('',#1984,#1935,#1028,.T.);
#2516=EDGE_CURVE('',#1931,#1985,#1234,.T.);
#2517=EDGE_CURVE('',#1985,#1937,#1029,.T.);
#2518=EDGE_CURVE('',#1985,#1983,#1030,.T.);
#2519=EDGE_CURVE('',#1984,#1936,#1031,.T.);
#2520=EDGE_CURVE('',#1984,#1986,#1708,.T.);
#2521=EDGE_CURVE('',#1987,#1986,#1709,.T.);
#2522=EDGE_CURVE('',#1987,#1950,#1710,.T.);
#2523=EDGE_CURVE('',#1988,#1983,#1711,.T.);
#2524=EDGE_CURVE('',#1989,#1988,#1712,.T.);
#2525=EDGE_CURVE('',#1989,#1980,#293,.T.);
#2526=EDGE_CURVE('',#1986,#1989,#1713,.T.);
#2527=EDGE_CURVE('',#1985,#1990,#1714,.T.);
#2528=EDGE_CURVE('',#1990,#1991,#1715,.T.);
#2529=EDGE_CURVE('',#1991,#1988,#1716,.T.);
#2530=EDGE_CURVE('',#1990,#1944,#1235,.T.);
#2531=EDGE_CURVE('',#1949,#1992,#1717,.T.);
#2532=EDGE_CURVE('',#1992,#1993,#1718,.T.);
#2533=EDGE_CURVE('',#1943,#1993,#1719,.T.);
#2534=EDGE_CURVE('',#1994,#1987,#1720,.T.);
#2535=EDGE_CURVE('',#1995,#1994,#1721,.T.);
#2536=EDGE_CURVE('',#1995,#1991,#1722,.T.);
#2537=EDGE_CURVE('',#1996,#1997,#1032,.T.);
#2538=EDGE_CURVE('',#1997,#1996,#1033,.T.);
#2539=EDGE_CURVE('',#1996,#1998,#1236,.T.);
#2540=EDGE_CURVE('',#1998,#1998,#1034,.T.);
#2541=EDGE_CURVE('',#1999,#2000,#1035,.T.);
#2542=EDGE_CURVE('',#2000,#1999,#1036,.T.);
#2543=EDGE_CURVE('',#2000,#1997,#1237,.T.);
#2544=EDGE_CURVE('',#2001,#2001,#1037,.T.);
#2545=EDGE_CURVE('',#2002,#2002,#1038,.T.);
#2546=EDGE_CURVE('',#2002,#1999,#1238,.T.);
#2547=EDGE_CURVE('',#2003,#2003,#1039,.T.);
#2548=EDGE_CURVE('',#2004,#2005,#1239,.T.);
#2549=EDGE_CURVE('',#2006,#2004,#1040,.T.);
#2550=EDGE_CURVE('',#2007,#2006,#1240,.T.);
#2551=EDGE_CURVE('',#2007,#2005,#1041,.T.);
#2552=EDGE_CURVE('',#2008,#2009,#1241,.T.);
#2553=EDGE_CURVE('',#2008,#2010,#1042,.T.);
#2554=EDGE_CURVE('',#2011,#2010,#1242,.T.);
#2555=EDGE_CURVE('',#2009,#2011,#1043,.T.);
#2556=EDGE_CURVE('',#2005,#2012,#1243,.T.);
#2557=EDGE_CURVE('',#2012,#2007,#1244,.T.);
#2558=EDGE_CURVE('',#2013,#2008,#1245,.T.);
#2559=EDGE_CURVE('',#2010,#2013,#1246,.T.);
#2560=EDGE_CURVE('',#2014,#2004,#1247,.T.);
#2561=EDGE_CURVE('',#2006,#2014,#1248,.T.);
#2562=EDGE_CURVE('',#2009,#2015,#1249,.T.);
#2563=EDGE_CURVE('',#2015,#2011,#1250,.T.);
#2564=EDGE_CURVE('',#2016,#2013,#1251,.T.);
#2565=EDGE_CURVE('',#2017,#2016,#1252,.T.);
#2566=EDGE_CURVE('',#2018,#2017,#1723,.T.);
#2567=EDGE_CURVE('',#2019,#2018,#1253,.T.);
#2568=EDGE_CURVE('',#2020,#2019,#1254,.T.);
#2569=EDGE_CURVE('',#2021,#2020,#1724,.T.);
#2570=EDGE_CURVE('',#2021,#2022,#1725,.T.);
#2571=EDGE_CURVE('',#2023,#2022,#1726,.T.);
#2572=EDGE_CURVE('',#2023,#2024,#1255,.T.);
#2573=EDGE_CURVE('',#2025,#2024,#1727,.F.);
#2574=EDGE_CURVE('',#2015,#2025,#1256,.T.);
#2575=EDGE_CURVE('',#2026,#2027,#1728,.T.);
#2576=EDGE_CURVE('',#2026,#2025,#1729,.T.);
#2577=EDGE_CURVE('',#2024,#2027,#1730,.T.);
#2578=EDGE_CURVE('',#2028,#2029,#1044,.T.);
#2579=EDGE_CURVE('',#2029,#2028,#1045,.T.);
#2580=EDGE_CURVE('',#2028,#2030,#1046,.T.);
#2581=EDGE_CURVE('',#2030,#2031,#1047,.T.);
#2582=EDGE_CURVE('',#2031,#2030,#1048,.T.);
#2583=EDGE_CURVE('',#2031,#2003,#1257,.T.);
#2584=EDGE_CURVE('',#2032,#2033,#1049,.T.);
#2585=EDGE_CURVE('',#2032,#2029,#1258,.T.);
#2586=EDGE_CURVE('',#2033,#2032,#1050,.T.);
#2587=EDGE_CURVE('',#2001,#2034,#1051,.T.);
#2588=EDGE_CURVE('',#2034,#2035,#1052,.T.);
#2589=EDGE_CURVE('',#2035,#2034,#1053,.T.);
#2590=EDGE_CURVE('',#2035,#2036,#1259,.T.);
#2591=EDGE_CURVE('',#2037,#2036,#1054,.T.);
#2592=EDGE_CURVE('',#2027,#2037,#1260,.T.);
#2593=EDGE_CURVE('',#2036,#2023,#1055,.T.);
#2594=EDGE_CURVE('',#2038,#2037,#1731,.T.);
#2595=EDGE_CURVE('',#2022,#2039,#1732,.T.);
#2596=EDGE_CURVE('',#2039,#2040,#1733,.T.);
#2597=EDGE_CURVE('',#2040,#2041,#1056,.T.);
#2598=EDGE_CURVE('',#2041,#2042,#1734,.T.);
#2599=EDGE_CURVE('',#2042,#2038,#1735,.T.);
#2600=EDGE_CURVE('',#2043,#2040,#1736,.T.);
#2601=EDGE_CURVE('',#2044,#2043,#1057,.T.);
#2602=EDGE_CURVE('',#2041,#2044,#1737,.T.);
#2603=EDGE_CURVE('',#2021,#2039,#1738,.T.);
#2604=EDGE_CURVE('',#2020,#2043,#1058,.T.);
#2605=EDGE_CURVE('',#2045,#2042,#1739,.F.);
#2606=EDGE_CURVE('',#2038,#2045,#1740,.T.);
#2607=EDGE_CURVE('',#2044,#2046,#1059,.T.);
#2608=EDGE_CURVE('',#2046,#2045,#1741,.T.);
#2609=EDGE_CURVE('',#2043,#2047,#1060,.T.);
#2610=EDGE_CURVE('',#2047,#2048,#1061,.T.);
#2611=EDGE_CURVE('',#2048,#2044,#1062,.T.);
#2612=EDGE_CURVE('',#2048,#2046,#1063,.T.);
#2613=EDGE_CURVE('',#2020,#2047,#1064,.T.);
#2614=EDGE_CURVE('',#2026,#2014,#1261,.T.);
#2615=EDGE_CURVE('',#2049,#2046,#1262,.T.);
#2616=EDGE_CURVE('',#2050,#2049,#1263,.T.);
#2617=EDGE_CURVE('',#2051,#2050,#1742,.T.);
#2618=EDGE_CURVE('',#2052,#2051,#1264,.T.);
#2619=EDGE_CURVE('',#2012,#2052,#1265,.T.);
#2620=EDGE_CURVE('',#2048,#2053,#1266,.T.);
#2621=EDGE_CURVE('',#2053,#2049,#1065,.F.);
#2622=EDGE_CURVE('',#2054,#2047,#1267,.T.);
#2623=EDGE_CURVE('',#2053,#2054,#1066,.T.);
#2624=EDGE_CURVE('',#2019,#2054,#1067,.F.);
#2625=EDGE_CURVE('',#2055,#2055,#1068,.T.);
#2626=EDGE_CURVE('',#2055,#2033,#1069,.T.);
#2627=EDGE_CURVE('',#2056,#2056,#1070,.T.);
#2628=EDGE_CURVE('',#2057,#2058,#1071,.T.);
#2629=EDGE_CURVE('',#2058,#2057,#1072,.T.);
#2630=EDGE_CURVE('',#2057,#2056,#1073,.T.);
#2631=EDGE_CURVE('',#2058,#2059,#1268,.T.);
#2632=EDGE_CURVE('',#2060,#2059,#1074,.T.);
#2633=EDGE_CURVE('',#2061,#2060,#1269,.T.);
#2634=EDGE_CURVE('',#2062,#2061,#1075,.T.);
#2635=EDGE_CURVE('',#2063,#2062,#1270,.T.);
#2636=EDGE_CURVE('',#2059,#2063,#1076,.T.);
#2637=EDGE_CURVE('',#2052,#2016,#1271,.T.);
#2638=EDGE_CURVE('',#2049,#2063,#1077,.F.);
#2639=EDGE_CURVE('',#2063,#2053,#1078,.F.);
#2640=EDGE_CURVE('',#2060,#2019,#1079,.F.);
#2641=EDGE_CURVE('',#2054,#2060,#1080,.F.);
#2642=EDGE_CURVE('',#2062,#2050,#1743,.T.);
#2643=EDGE_CURVE('',#2061,#2018,#1744,.T.);
#2644=EDGE_CURVE('',#2017,#2051,#1081,.T.);
#2645=EDGE_CURVE('',#2064,#2064,#1082,.T.);
#2646=EDGE_CURVE('',#2064,#2065,#1083,.T.);
#2647=EDGE_CURVE('',#2065,#2066,#1084,.T.);
#2648=EDGE_CURVE('',#2066,#2065,#1085,.T.);
#2649=EDGE_CURVE('',#2066,#2067,#1272,.T.);
#2650=EDGE_CURVE('',#2068,#2067,#1086,.T.);
#2651=EDGE_CURVE('',#2067,#2068,#1087,.T.);
#2652=EDGE_CURVE('',#2069,#2069,#1088,.T.);
#2653=EDGE_CURVE('',#2068,#2070,#1089,.T.);
#2654=EDGE_CURVE('',#2070,#2071,#1090,.T.);
#2655=EDGE_CURVE('',#2071,#2070,#1091,.T.);
#2656=EDGE_CURVE('',#2071,#2072,#1273,.T.);
#2657=EDGE_CURVE('',#2073,#2072,#1092,.T.);
#2658=EDGE_CURVE('',#2072,#2073,#1093,.T.);
#2659=EDGE_CURVE('',#2073,#2074,#1094,.T.);
#2660=EDGE_CURVE('',#2074,#2074,#1095,.T.);
#2661=EDGE_CURVE('',#2075,#2075,#1096,.T.);
#2662=EDGE_CURVE('',#2075,#2076,#1097,.T.);
#2663=EDGE_CURVE('',#2076,#2077,#1098,.T.);
#2664=EDGE_CURVE('',#2077,#2076,#1099,.T.);
#2665=EDGE_CURVE('',#2078,#2079,#1100,.T.);
#2666=EDGE_CURVE('',#2079,#2078,#1101,.T.);
#2667=EDGE_CURVE('',#2079,#2077,#1274,.T.);
#2668=EDGE_CURVE('',#2078,#2069,#1102,.T.);
#2669=EDGE_CURVE('',#2080,#2080,#1103,.T.);
#2670=EDGE_CURVE('',#2080,#2081,#1275,.T.);
#2671=EDGE_CURVE('',#2081,#2081,#1104,.T.);
#2672=EDGE_CURVE('',#2082,#2082,#1105,.T.);
#2673=EDGE_CURVE('',#2082,#2083,#1276,.T.);
#2674=EDGE_CURVE('',#2083,#2083,#1106,.T.);
#2675=EDGE_CURVE('',#2083,#2084,#1277,.T.);
#2676=EDGE_CURVE('',#2084,#2084,#1107,.T.);
#2677=EDGE_CURVE('',#2084,#2085,#1278,.T.);
#2678=EDGE_CURVE('',#2085,#2085,#1108,.T.);
#2679=EDGE_CURVE('',#2086,#2086,#1109,.T.);
#2680=EDGE_CURVE('',#2086,#2087,#1279,.T.);
#2681=EDGE_CURVE('',#2087,#2087,#1110,.T.);
#2682=EDGE_CURVE('',#2088,#2088,#1111,.T.);
#2683=EDGE_CURVE('',#2088,#2086,#1280,.T.);
#2684=EDGE_CURVE('',#2089,#2089,#1112,.T.);
#2685=EDGE_CURVE('',#2089,#2088,#1281,.T.);
#2686=EDGE_CURVE('',#2090,#2090,#1113,.T.);
#2687=EDGE_CURVE('',#2090,#2091,#1282,.T.);
#2688=EDGE_CURVE('',#2091,#2091,#1114,.T.);
#2689=EDGE_CURVE('',#2092,#2092,#1115,.T.);
#2690=EDGE_CURVE('',#2092,#2093,#1283,.T.);
#2691=EDGE_CURVE('',#2093,#2093,#1116,.T.);
#2692=EDGE_CURVE('',#2094,#2094,#1117,.T.);
#2693=EDGE_CURVE('',#2094,#2095,#1284,.T.);
#2694=EDGE_CURVE('',#2095,#2095,#1118,.T.);
#2695=EDGE_CURVE('',#2096,#2097,#1285,.T.);
#2696=EDGE_CURVE('',#2097,#2098,#1286,.T.);
#2697=EDGE_CURVE('',#2098,#2099,#1287,.T.);
#2698=EDGE_CURVE('',#2099,#2100,#1119,.T.);
#2699=EDGE_CURVE('',#2100,#2101,#1288,.T.);
#2700=EDGE_CURVE('',#2101,#2102,#1289,.T.);
#2701=EDGE_CURVE('',#2102,#2103,#1290,.T.);
#2702=EDGE_CURVE('',#2096,#2103,#1120,.T.);
#2703=EDGE_CURVE('',#2104,#2102,#1291,.T.);
#2704=EDGE_CURVE('',#2105,#2104,#1292,.T.);
#2705=EDGE_CURVE('',#2103,#2105,#1293,.T.);
#2706=EDGE_CURVE('',#2104,#2106,#1294,.T.);
#2707=EDGE_CURVE('',#2106,#2101,#1295,.T.);
#2708=EDGE_CURVE('',#2107,#2100,#1296,.T.);
#2709=EDGE_CURVE('',#2106,#2107,#1297,.T.);
#2710=EDGE_CURVE('',#2108,#2109,#1298,.T.);
#2711=EDGE_CURVE('',#2109,#2105,#1121,.T.);
#2712=EDGE_CURVE('',#2110,#2107,#1122,.T.);
#2713=EDGE_CURVE('',#2111,#2110,#1299,.T.);
#2714=EDGE_CURVE('',#2108,#2111,#1300,.T.);
#2715=EDGE_CURVE('',#2099,#2110,#1301,.T.);
#2716=EDGE_CURVE('',#2111,#2098,#1302,.T.);
#2717=EDGE_CURVE('',#2108,#2097,#1303,.T.);
#2718=EDGE_CURVE('',#2109,#2096,#1304,.T.);
#2719=EDGE_CURVE('',#2112,#2113,#1305,.T.);
#2720=EDGE_CURVE('',#2114,#2112,#1306,.T.);
#2721=EDGE_CURVE('',#2113,#2114,#1307,.T.);
#2722=EDGE_CURVE('',#2115,#2116,#1308,.T.);
#2723=EDGE_CURVE('',#2117,#2115,#1309,.T.);
#2724=EDGE_CURVE('',#2116,#2117,#1310,.T.);
#2725=EDGE_CURVE('',#2118,#2119,#1311,.T.);
#2726=EDGE_CURVE('',#2120,#2118,#1312,.T.);
#2727=EDGE_CURVE('',#2119,#2120,#1313,.T.);
#2728=EDGE_CURVE('',#2121,#2122,#1314,.T.);
#2729=EDGE_CURVE('',#2123,#2121,#1315,.T.);
#2730=EDGE_CURVE('',#2122,#2123,#1316,.T.);
#2731=EDGE_CURVE('',#2112,#2123,#1317,.T.);
#2732=EDGE_CURVE('',#2121,#2114,#1318,.T.);
#2733=EDGE_CURVE('',#2124,#2125,#1319,.T.);
#2734=EDGE_CURVE('',#2126,#2124,#1320,.T.);
#2735=EDGE_CURVE('',#2125,#2126,#1321,.T.);
#2736=EDGE_CURVE('',#2127,#2128,#1322,.T.);
#2737=EDGE_CURVE('',#2129,#2127,#1323,.T.);
#2738=EDGE_CURVE('',#2128,#2129,#1324,.T.);
#2739=EDGE_CURVE('',#2115,#2129,#1325,.T.);
#2740=EDGE_CURVE('',#2127,#2117,#1326,.T.);
#2741=EDGE_CURVE('',#2130,#2131,#1327,.T.);
#2742=EDGE_CURVE('',#2132,#2130,#1328,.T.);
#2743=EDGE_CURVE('',#2131,#2132,#1329,.T.);
#2744=EDGE_CURVE('',#2130,#2120,#1330,.T.);
#2745=EDGE_CURVE('',#2118,#2132,#1331,.T.);
#2746=EDGE_CURVE('',#2122,#2131,#1332,.T.);
#2747=EDGE_CURVE('',#2132,#2121,#1333,.T.);
#2748=EDGE_CURVE('',#2133,#2134,#1334,.T.);
#2749=EDGE_CURVE('',#2135,#2133,#1335,.T.);
#2750=EDGE_CURVE('',#2134,#2135,#1336,.T.);
#2751=EDGE_CURVE('',#2124,#2135,#1337,.T.);
#2752=EDGE_CURVE('',#2133,#2126,#1338,.T.);
#2753=EDGE_CURVE('',#2131,#2134,#1339,.T.);
#2754=EDGE_CURVE('',#2135,#2130,#1340,.T.);
#2755=EDGE_CURVE('',#2134,#2128,#1341,.T.);
#2756=EDGE_CURVE('',#2129,#2133,#1342,.T.);
#2757=EDGE_CURVE('',#2128,#2122,#1343,.T.);
#2758=EDGE_CURVE('',#2123,#2127,#1344,.T.);
#2759=EDGE_CURVE('',#2116,#2125,#1345,.T.);
#2760=EDGE_CURVE('',#2126,#2115,#1346,.T.);
#2761=EDGE_CURVE('',#2125,#2119,#1347,.T.);
#2762=EDGE_CURVE('',#2120,#2124,#1348,.T.);
#2763=EDGE_CURVE('',#2119,#2113,#1349,.T.);
#2764=EDGE_CURVE('',#2114,#2118,#1350,.T.);
#2765=EDGE_CURVE('',#2113,#2116,#1351,.T.);
#2766=EDGE_CURVE('',#2117,#2112,#1352,.T.);
#2767=ORIENTED_EDGE('',*,*,#2136,.F.);
#2768=ORIENTED_EDGE('',*,*,#2137,.F.);
#2769=ORIENTED_EDGE('',*,*,#2138,.T.);
#2770=ORIENTED_EDGE('',*,*,#2139,.F.);
#2771=ORIENTED_EDGE('',*,*,#2140,.F.);
#2772=ORIENTED_EDGE('',*,*,#2138,.F.);
#2773=ORIENTED_EDGE('',*,*,#2136,.T.);
#2774=ORIENTED_EDGE('',*,*,#2137,.T.);
#2775=ORIENTED_EDGE('',*,*,#2141,.F.);
#2776=ORIENTED_EDGE('',*,*,#2142,.T.);
#2777=ORIENTED_EDGE('',*,*,#2141,.T.);
#2778=ORIENTED_EDGE('',*,*,#2142,.F.);
#2779=ORIENTED_EDGE('',*,*,#2143,.F.);
#2780=ORIENTED_EDGE('',*,*,#2144,.F.);
#2781=ORIENTED_EDGE('',*,*,#2143,.T.);
#2782=ORIENTED_EDGE('',*,*,#2140,.T.);
#2783=ORIENTED_EDGE('',*,*,#2145,.T.);
#2784=ORIENTED_EDGE('',*,*,#2146,.T.);
#2785=ORIENTED_EDGE('',*,*,#2145,.F.);
#2786=ORIENTED_EDGE('',*,*,#2139,.T.);
#2787=ORIENTED_EDGE('',*,*,#2147,.F.);
#2788=ORIENTED_EDGE('',*,*,#2146,.F.);
#2789=ORIENTED_EDGE('',*,*,#2148,.T.);
#2790=ORIENTED_EDGE('',*,*,#2149,.T.);
#2791=ORIENTED_EDGE('',*,*,#2148,.F.);
#2792=ORIENTED_EDGE('',*,*,#2147,.T.);
#2793=ORIENTED_EDGE('',*,*,#2149,.F.);
#2794=ORIENTED_EDGE('',*,*,#2150,.T.);
#2795=ORIENTED_EDGE('',*,*,#2151,.F.);
#2796=ORIENTED_EDGE('',*,*,#2150,.F.);
#2797=ORIENTED_EDGE('',*,*,#2152,.T.);
#2798=ORIENTED_EDGE('',*,*,#2153,.T.);
#2799=ORIENTED_EDGE('',*,*,#2152,.F.);
#2800=ORIENTED_EDGE('',*,*,#2151,.T.);
#2801=ORIENTED_EDGE('',*,*,#2154,.T.);
#2802=ORIENTED_EDGE('',*,*,#2155,.T.);
#2803=ORIENTED_EDGE('',*,*,#2153,.F.);
#2804=ORIENTED_EDGE('',*,*,#2156,.T.);
#2805=ORIENTED_EDGE('',*,*,#2144,.T.);
#2806=ORIENTED_EDGE('',*,*,#2156,.F.);
#2807=ORIENTED_EDGE('',*,*,#2157,.T.);
#2808=ORIENTED_EDGE('',*,*,#2158,.F.);
#2809=ORIENTED_EDGE('',*,*,#2157,.F.);
#2810=ORIENTED_EDGE('',*,*,#2159,.T.);
#2811=ORIENTED_EDGE('',*,*,#2160,.T.);
#2812=ORIENTED_EDGE('',*,*,#2161,.T.);
#2813=ORIENTED_EDGE('',*,*,#2162,.T.);
#2814=ORIENTED_EDGE('',*,*,#2163,.T.);
#2815=ORIENTED_EDGE('',*,*,#2164,.T.);
#2816=ORIENTED_EDGE('',*,*,#2165,.T.);
#2817=ORIENTED_EDGE('',*,*,#2161,.F.);
#2818=ORIENTED_EDGE('',*,*,#2166,.T.);
#2819=ORIENTED_EDGE('',*,*,#2167,.T.);
#2820=ORIENTED_EDGE('',*,*,#2168,.T.);
#2821=ORIENTED_EDGE('',*,*,#2164,.F.);
#2822=ORIENTED_EDGE('',*,*,#2169,.T.);
#2823=ORIENTED_EDGE('',*,*,#2170,.T.);
#2824=ORIENTED_EDGE('',*,*,#2171,.T.);
#2825=ORIENTED_EDGE('',*,*,#2167,.F.);
#2826=ORIENTED_EDGE('',*,*,#2172,.T.);
#2827=ORIENTED_EDGE('',*,*,#2173,.F.);
#2828=ORIENTED_EDGE('',*,*,#2174,.T.);
#2829=ORIENTED_EDGE('',*,*,#2170,.F.);
#2830=ORIENTED_EDGE('',*,*,#2175,.T.);
#2831=ORIENTED_EDGE('',*,*,#2175,.F.);
#2832=ORIENTED_EDGE('',*,*,#2172,.F.);
#2833=ORIENTED_EDGE('',*,*,#2169,.F.);
#2834=ORIENTED_EDGE('',*,*,#2166,.F.);
#2835=ORIENTED_EDGE('',*,*,#2160,.F.);
#2836=ORIENTED_EDGE('',*,*,#2176,.F.);
#2837=ORIENTED_EDGE('',*,*,#2177,.F.);
#2838=ORIENTED_EDGE('',*,*,#2178,.T.);
#2839=ORIENTED_EDGE('',*,*,#2179,.T.);
#2840=ORIENTED_EDGE('',*,*,#2180,.T.);
#2841=ORIENTED_EDGE('',*,*,#2181,.T.);
#2842=ORIENTED_EDGE('',*,*,#2182,.T.);
#2843=ORIENTED_EDGE('',*,*,#2183,.T.);
#2844=ORIENTED_EDGE('',*,*,#2180,.F.);
#2845=ORIENTED_EDGE('',*,*,#2184,.T.);
#2846=ORIENTED_EDGE('',*,*,#2185,.T.);
#2847=ORIENTED_EDGE('',*,*,#2186,.T.);
#2848=ORIENTED_EDGE('',*,*,#2182,.F.);
#2849=ORIENTED_EDGE('',*,*,#2187,.T.);
#2850=ORIENTED_EDGE('',*,*,#2188,.T.);
#2851=ORIENTED_EDGE('',*,*,#2189,.T.);
#2852=ORIENTED_EDGE('',*,*,#2185,.F.);
#2853=ORIENTED_EDGE('',*,*,#2190,.T.);
#2854=ORIENTED_EDGE('',*,*,#2191,.F.);
#2855=ORIENTED_EDGE('',*,*,#2192,.T.);
#2856=ORIENTED_EDGE('',*,*,#2188,.F.);
#2857=ORIENTED_EDGE('',*,*,#2193,.T.);
#2858=ORIENTED_EDGE('',*,*,#2194,.F.);
#2859=ORIENTED_EDGE('',*,*,#2193,.F.);
#2860=ORIENTED_EDGE('',*,*,#2190,.F.);
#2861=ORIENTED_EDGE('',*,*,#2187,.F.);
#2862=ORIENTED_EDGE('',*,*,#2184,.F.);
#2863=ORIENTED_EDGE('',*,*,#2179,.F.);
#2864=ORIENTED_EDGE('',*,*,#2195,.F.);
#2865=ORIENTED_EDGE('',*,*,#2196,.F.);
#2866=ORIENTED_EDGE('',*,*,#2197,.T.);
#2867=ORIENTED_EDGE('',*,*,#2163,.F.);
#2868=ORIENTED_EDGE('',*,*,#2198,.T.);
#2869=ORIENTED_EDGE('',*,*,#2191,.T.);
#2870=ORIENTED_EDGE('',*,*,#2197,.F.);
#2871=ORIENTED_EDGE('',*,*,#2194,.T.);
#2872=ORIENTED_EDGE('',*,*,#2196,.T.);
#2873=ORIENTED_EDGE('',*,*,#2199,.F.);
#2874=ORIENTED_EDGE('',*,*,#2176,.T.);
#2875=ORIENTED_EDGE('',*,*,#2159,.F.);
#2876=ORIENTED_EDGE('',*,*,#2177,.T.);
#2877=ORIENTED_EDGE('',*,*,#2199,.T.);
#2878=ORIENTED_EDGE('',*,*,#2195,.T.);
#2879=ORIENTED_EDGE('',*,*,#2178,.F.);
#2880=ORIENTED_EDGE('',*,*,#2154,.F.);
#2881=ORIENTED_EDGE('',*,*,#2173,.T.);
#2882=ORIENTED_EDGE('',*,*,#2174,.F.);
#2883=ORIENTED_EDGE('',*,*,#2155,.F.);
#2884=ORIENTED_EDGE('',*,*,#2181,.F.);
#2885=ORIENTED_EDGE('',*,*,#2200,.F.);
#2886=ORIENTED_EDGE('',*,*,#2171,.F.);
#2887=ORIENTED_EDGE('',*,*,#2200,.T.);
#2888=ORIENTED_EDGE('',*,*,#2183,.F.);
#2889=ORIENTED_EDGE('',*,*,#2201,.T.);
#2890=ORIENTED_EDGE('',*,*,#2168,.F.);
#2891=ORIENTED_EDGE('',*,*,#2201,.F.);
#2892=ORIENTED_EDGE('',*,*,#2186,.F.);
#2893=ORIENTED_EDGE('',*,*,#2202,.F.);
#2894=ORIENTED_EDGE('',*,*,#2162,.F.);
#2895=ORIENTED_EDGE('',*,*,#2203,.F.);
#2896=ORIENTED_EDGE('',*,*,#2204,.T.);
#2897=ORIENTED_EDGE('',*,*,#2205,.F.);
#2898=ORIENTED_EDGE('',*,*,#2206,.F.);
#2899=ORIENTED_EDGE('',*,*,#2204,.F.);
#2900=ORIENTED_EDGE('',*,*,#2207,.F.);
#2901=ORIENTED_EDGE('',*,*,#2192,.F.);
#2902=ORIENTED_EDGE('',*,*,#2198,.F.);
#2903=ORIENTED_EDGE('',*,*,#2165,.F.);
#2904=ORIENTED_EDGE('',*,*,#2202,.T.);
#2905=ORIENTED_EDGE('',*,*,#2189,.F.);
#2906=ORIENTED_EDGE('',*,*,#2207,.T.);
#2907=ORIENTED_EDGE('',*,*,#2203,.T.);
#2908=ORIENTED_EDGE('',*,*,#2205,.T.);
#2909=ORIENTED_EDGE('',*,*,#2206,.T.);
#2910=ORIENTED_EDGE('',*,*,#2208,.T.);
#2911=ORIENTED_EDGE('',*,*,#2158,.T.);
#2912=ORIENTED_EDGE('',*,*,#2208,.F.);
#2913=ORIENTED_EDGE('',*,*,#2209,.T.);
#2914=ORIENTED_EDGE('',*,*,#2210,.T.);
#2915=ORIENTED_EDGE('',*,*,#2211,.T.);
#2916=ORIENTED_EDGE('',*,*,#2212,.T.);
#2917=ORIENTED_EDGE('',*,*,#2210,.F.);
#2918=ORIENTED_EDGE('',*,*,#2212,.F.);
#2919=ORIENTED_EDGE('',*,*,#2213,.T.);
#2920=ORIENTED_EDGE('',*,*,#2214,.F.);
#2921=ORIENTED_EDGE('',*,*,#2215,.F.);
#2922=ORIENTED_EDGE('',*,*,#2213,.F.);
#2923=ORIENTED_EDGE('',*,*,#2211,.F.);
#2924=ORIENTED_EDGE('',*,*,#2209,.F.);
#2925=ORIENTED_EDGE('',*,*,#2216,.F.);
#2926=ORIENTED_EDGE('',*,*,#2214,.T.);
#2927=ORIENTED_EDGE('',*,*,#2215,.T.);
#2928=ORIENTED_EDGE('',*,*,#2217,.T.);
#2929=ORIENTED_EDGE('',*,*,#2218,.T.);
#2930=ORIENTED_EDGE('',*,*,#2219,.T.);
#2931=ORIENTED_EDGE('',*,*,#2217,.F.);
#2932=ORIENTED_EDGE('',*,*,#2219,.F.);
#2933=ORIENTED_EDGE('',*,*,#2220,.T.);
#2934=ORIENTED_EDGE('',*,*,#2221,.F.);
#2935=ORIENTED_EDGE('',*,*,#2222,.F.);
#2936=ORIENTED_EDGE('',*,*,#2220,.F.);
#2937=ORIENTED_EDGE('',*,*,#2218,.F.);
#2938=ORIENTED_EDGE('',*,*,#2221,.T.);
#2939=ORIENTED_EDGE('',*,*,#2222,.T.);
#2940=ORIENTED_EDGE('',*,*,#2223,.T.);
#2941=ORIENTED_EDGE('',*,*,#2224,.T.);
#2942=ORIENTED_EDGE('',*,*,#2225,.T.);
#2943=ORIENTED_EDGE('',*,*,#2223,.F.);
#2944=ORIENTED_EDGE('',*,*,#2225,.F.);
#2945=ORIENTED_EDGE('',*,*,#2226,.T.);
#2946=ORIENTED_EDGE('',*,*,#2227,.F.);
#2947=ORIENTED_EDGE('',*,*,#2228,.F.);
#2948=ORIENTED_EDGE('',*,*,#2226,.F.);
#2949=ORIENTED_EDGE('',*,*,#2224,.F.);
#2950=ORIENTED_EDGE('',*,*,#2227,.T.);
#2951=ORIENTED_EDGE('',*,*,#2228,.T.);
#2952=ORIENTED_EDGE('',*,*,#2229,.T.);
#2953=ORIENTED_EDGE('',*,*,#2230,.T.);
#2954=ORIENTED_EDGE('',*,*,#2231,.T.);
#2955=ORIENTED_EDGE('',*,*,#2229,.F.);
#2956=ORIENTED_EDGE('',*,*,#2231,.F.);
#2957=ORIENTED_EDGE('',*,*,#2232,.T.);
#2958=ORIENTED_EDGE('',*,*,#2233,.F.);
#2959=ORIENTED_EDGE('',*,*,#2234,.F.);
#2960=ORIENTED_EDGE('',*,*,#2232,.F.);
#2961=ORIENTED_EDGE('',*,*,#2230,.F.);
#2962=ORIENTED_EDGE('',*,*,#2233,.T.);
#2963=ORIENTED_EDGE('',*,*,#2234,.T.);
#2964=ORIENTED_EDGE('',*,*,#2235,.T.);
#2965=ORIENTED_EDGE('',*,*,#2236,.T.);
#2966=ORIENTED_EDGE('',*,*,#2237,.T.);
#2967=ORIENTED_EDGE('',*,*,#2235,.F.);
#2968=ORIENTED_EDGE('',*,*,#2237,.F.);
#2969=ORIENTED_EDGE('',*,*,#2238,.T.);
#2970=ORIENTED_EDGE('',*,*,#2239,.F.);
#2971=ORIENTED_EDGE('',*,*,#2240,.F.);
#2972=ORIENTED_EDGE('',*,*,#2238,.F.);
#2973=ORIENTED_EDGE('',*,*,#2236,.F.);
#2974=ORIENTED_EDGE('',*,*,#2239,.T.);
#2975=ORIENTED_EDGE('',*,*,#2240,.T.);
#2976=ORIENTED_EDGE('',*,*,#2241,.T.);
#2977=ORIENTED_EDGE('',*,*,#2242,.T.);
#2978=ORIENTED_EDGE('',*,*,#2241,.F.);
#2979=ORIENTED_EDGE('',*,*,#2242,.F.);
#2980=ORIENTED_EDGE('',*,*,#2243,.F.);
#2981=ORIENTED_EDGE('',*,*,#2243,.T.);
#2982=ORIENTED_EDGE('',*,*,#2244,.T.);
#2983=ORIENTED_EDGE('',*,*,#2245,.T.);
#2984=ORIENTED_EDGE('',*,*,#2246,.T.);
#2985=ORIENTED_EDGE('',*,*,#2244,.F.);
#2986=ORIENTED_EDGE('',*,*,#2247,.F.);
#2987=ORIENTED_EDGE('',*,*,#2248,.F.);
#2988=ORIENTED_EDGE('',*,*,#2249,.T.);
#2989=ORIENTED_EDGE('',*,*,#2245,.F.);
#2990=ORIENTED_EDGE('',*,*,#2246,.F.);
#2991=ORIENTED_EDGE('',*,*,#2249,.F.);
#2992=ORIENTED_EDGE('',*,*,#2247,.T.);
#2993=ORIENTED_EDGE('',*,*,#2248,.T.);
#2994=ORIENTED_EDGE('',*,*,#2250,.T.);
#2995=ORIENTED_EDGE('',*,*,#2216,.T.);
#2996=ORIENTED_EDGE('',*,*,#2250,.F.);
#2997=ORIENTED_EDGE('',*,*,#2251,.T.);
#2998=ORIENTED_EDGE('',*,*,#2252,.T.);
#2999=ORIENTED_EDGE('',*,*,#2253,.T.);
#3000=ORIENTED_EDGE('',*,*,#2254,.T.);
#3001=ORIENTED_EDGE('',*,*,#2255,.T.);
#3002=ORIENTED_EDGE('',*,*,#2256,.T.);
#3003=ORIENTED_EDGE('',*,*,#2251,.F.);
#3004=ORIENTED_EDGE('',*,*,#2257,.T.);
#3005=ORIENTED_EDGE('',*,*,#2258,.T.);
#3006=ORIENTED_EDGE('',*,*,#2259,.T.);
#3007=ORIENTED_EDGE('',*,*,#2255,.F.);
#3008=ORIENTED_EDGE('',*,*,#2260,.T.);
#3009=ORIENTED_EDGE('',*,*,#2261,.T.);
#3010=ORIENTED_EDGE('',*,*,#2262,.T.);
#3011=ORIENTED_EDGE('',*,*,#2258,.F.);
#3012=ORIENTED_EDGE('',*,*,#2263,.T.);
#3013=ORIENTED_EDGE('',*,*,#2264,.T.);
#3014=ORIENTED_EDGE('',*,*,#2265,.T.);
#3015=ORIENTED_EDGE('',*,*,#2261,.F.);
#3016=ORIENTED_EDGE('',*,*,#2266,.T.);
#3017=ORIENTED_EDGE('',*,*,#2267,.T.);
#3018=ORIENTED_EDGE('',*,*,#2268,.T.);
#3019=ORIENTED_EDGE('',*,*,#2264,.F.);
#3020=ORIENTED_EDGE('',*,*,#2269,.T.);
#3021=ORIENTED_EDGE('',*,*,#2270,.T.);
#3022=ORIENTED_EDGE('',*,*,#2271,.T.);
#3023=ORIENTED_EDGE('',*,*,#2267,.F.);
#3024=ORIENTED_EDGE('',*,*,#2272,.T.);
#3025=ORIENTED_EDGE('',*,*,#2273,.T.);
#3026=ORIENTED_EDGE('',*,*,#2274,.T.);
#3027=ORIENTED_EDGE('',*,*,#2270,.F.);
#3028=ORIENTED_EDGE('',*,*,#2275,.T.);
#3029=ORIENTED_EDGE('',*,*,#2276,.T.);
#3030=ORIENTED_EDGE('',*,*,#2277,.T.);
#3031=ORIENTED_EDGE('',*,*,#2273,.F.);
#3032=ORIENTED_EDGE('',*,*,#2278,.T.);
#3033=ORIENTED_EDGE('',*,*,#2279,.T.);
#3034=ORIENTED_EDGE('',*,*,#2280,.T.);
#3035=ORIENTED_EDGE('',*,*,#2276,.F.);
#3036=ORIENTED_EDGE('',*,*,#2281,.T.);
#3037=ORIENTED_EDGE('',*,*,#2282,.T.);
#3038=ORIENTED_EDGE('',*,*,#2283,.T.);
#3039=ORIENTED_EDGE('',*,*,#2279,.F.);
#3040=ORIENTED_EDGE('',*,*,#2284,.T.);
#3041=ORIENTED_EDGE('',*,*,#2285,.T.);
#3042=ORIENTED_EDGE('',*,*,#2286,.T.);
#3043=ORIENTED_EDGE('',*,*,#2282,.F.);
#3044=ORIENTED_EDGE('',*,*,#2287,.T.);
#3045=ORIENTED_EDGE('',*,*,#2288,.T.);
#3046=ORIENTED_EDGE('',*,*,#2289,.T.);
#3047=ORIENTED_EDGE('',*,*,#2285,.F.);
#3048=ORIENTED_EDGE('',*,*,#2290,.T.);
#3049=ORIENTED_EDGE('',*,*,#2291,.T.);
#3050=ORIENTED_EDGE('',*,*,#2292,.T.);
#3051=ORIENTED_EDGE('',*,*,#2288,.F.);
#3052=ORIENTED_EDGE('',*,*,#2293,.T.);
#3053=ORIENTED_EDGE('',*,*,#2294,.T.);
#3054=ORIENTED_EDGE('',*,*,#2295,.T.);
#3055=ORIENTED_EDGE('',*,*,#2291,.F.);
#3056=ORIENTED_EDGE('',*,*,#2296,.T.);
#3057=ORIENTED_EDGE('',*,*,#2297,.T.);
#3058=ORIENTED_EDGE('',*,*,#2298,.T.);
#3059=ORIENTED_EDGE('',*,*,#2294,.F.);
#3060=ORIENTED_EDGE('',*,*,#2299,.T.);
#3061=ORIENTED_EDGE('',*,*,#2300,.F.);
#3062=ORIENTED_EDGE('',*,*,#2301,.T.);
#3063=ORIENTED_EDGE('',*,*,#2302,.F.);
#3064=ORIENTED_EDGE('',*,*,#2303,.T.);
#3065=ORIENTED_EDGE('',*,*,#2304,.T.);
#3066=ORIENTED_EDGE('',*,*,#2305,.T.);
#3067=ORIENTED_EDGE('',*,*,#2306,.F.);
#3068=ORIENTED_EDGE('',*,*,#2307,.F.);
#3069=ORIENTED_EDGE('',*,*,#2308,.T.);
#3070=ORIENTED_EDGE('',*,*,#2309,.T.);
#3071=ORIENTED_EDGE('',*,*,#2304,.F.);
#3072=ORIENTED_EDGE('',*,*,#2310,.F.);
#3073=ORIENTED_EDGE('',*,*,#2311,.T.);
#3074=ORIENTED_EDGE('',*,*,#2312,.T.);
#3075=ORIENTED_EDGE('',*,*,#2308,.F.);
#3076=ORIENTED_EDGE('',*,*,#2313,.F.);
#3077=ORIENTED_EDGE('',*,*,#2314,.T.);
#3078=ORIENTED_EDGE('',*,*,#2315,.T.);
#3079=ORIENTED_EDGE('',*,*,#2311,.F.);
#3080=ORIENTED_EDGE('',*,*,#2316,.F.);
#3081=ORIENTED_EDGE('',*,*,#2317,.T.);
#3082=ORIENTED_EDGE('',*,*,#2318,.T.);
#3083=ORIENTED_EDGE('',*,*,#2314,.F.);
#3084=ORIENTED_EDGE('',*,*,#2319,.F.);
#3085=ORIENTED_EDGE('',*,*,#2320,.T.);
#3086=ORIENTED_EDGE('',*,*,#2321,.T.);
#3087=ORIENTED_EDGE('',*,*,#2317,.F.);
#3088=ORIENTED_EDGE('',*,*,#2322,.F.);
#3089=ORIENTED_EDGE('',*,*,#2323,.T.);
#3090=ORIENTED_EDGE('',*,*,#2324,.T.);
#3091=ORIENTED_EDGE('',*,*,#2320,.F.);
#3092=ORIENTED_EDGE('',*,*,#2325,.F.);
#3093=ORIENTED_EDGE('',*,*,#2326,.T.);
#3094=ORIENTED_EDGE('',*,*,#2327,.T.);
#3095=ORIENTED_EDGE('',*,*,#2323,.F.);
#3096=ORIENTED_EDGE('',*,*,#2328,.F.);
#3097=ORIENTED_EDGE('',*,*,#2329,.T.);
#3098=ORIENTED_EDGE('',*,*,#2330,.T.);
#3099=ORIENTED_EDGE('',*,*,#2326,.F.);
#3100=ORIENTED_EDGE('',*,*,#2331,.F.);
#3101=ORIENTED_EDGE('',*,*,#2332,.T.);
#3102=ORIENTED_EDGE('',*,*,#2333,.T.);
#3103=ORIENTED_EDGE('',*,*,#2329,.F.);
#3104=ORIENTED_EDGE('',*,*,#2334,.F.);
#3105=ORIENTED_EDGE('',*,*,#2335,.T.);
#3106=ORIENTED_EDGE('',*,*,#2336,.T.);
#3107=ORIENTED_EDGE('',*,*,#2332,.F.);
#3108=ORIENTED_EDGE('',*,*,#2337,.F.);
#3109=ORIENTED_EDGE('',*,*,#2338,.T.);
#3110=ORIENTED_EDGE('',*,*,#2339,.T.);
#3111=ORIENTED_EDGE('',*,*,#2335,.F.);
#3112=ORIENTED_EDGE('',*,*,#2340,.F.);
#3113=ORIENTED_EDGE('',*,*,#2341,.T.);
#3114=ORIENTED_EDGE('',*,*,#2342,.T.);
#3115=ORIENTED_EDGE('',*,*,#2338,.F.);
#3116=ORIENTED_EDGE('',*,*,#2343,.F.);
#3117=ORIENTED_EDGE('',*,*,#2344,.T.);
#3118=ORIENTED_EDGE('',*,*,#2345,.T.);
#3119=ORIENTED_EDGE('',*,*,#2341,.F.);
#3120=ORIENTED_EDGE('',*,*,#2346,.F.);
#3121=ORIENTED_EDGE('',*,*,#2347,.T.);
#3122=ORIENTED_EDGE('',*,*,#2348,.T.);
#3123=ORIENTED_EDGE('',*,*,#2344,.F.);
#3124=ORIENTED_EDGE('',*,*,#2349,.F.);
#3125=ORIENTED_EDGE('',*,*,#2350,.T.);
#3126=ORIENTED_EDGE('',*,*,#2351,.T.);
#3127=ORIENTED_EDGE('',*,*,#2347,.F.);
#3128=ORIENTED_EDGE('',*,*,#2352,.F.);
#3129=ORIENTED_EDGE('',*,*,#2353,.T.);
#3130=ORIENTED_EDGE('',*,*,#2354,.T.);
#3131=ORIENTED_EDGE('',*,*,#2350,.F.);
#3132=ORIENTED_EDGE('',*,*,#2355,.F.);
#3133=ORIENTED_EDGE('',*,*,#2356,.F.);
#3134=ORIENTED_EDGE('',*,*,#2357,.F.);
#3135=ORIENTED_EDGE('',*,*,#2358,.F.);
#3136=ORIENTED_EDGE('',*,*,#2359,.T.);
#3137=ORIENTED_EDGE('',*,*,#2360,.T.);
#3138=ORIENTED_EDGE('',*,*,#2361,.T.);
#3139=ORIENTED_EDGE('',*,*,#2362,.T.);
#3140=ORIENTED_EDGE('',*,*,#2306,.T.);
#3141=ORIENTED_EDGE('',*,*,#2363,.T.);
#3142=ORIENTED_EDGE('',*,*,#2356,.T.);
#3143=ORIENTED_EDGE('',*,*,#2364,.T.);
#3144=ORIENTED_EDGE('',*,*,#2353,.F.);
#3145=ORIENTED_EDGE('',*,*,#2365,.F.);
#3146=ORIENTED_EDGE('',*,*,#2363,.F.);
#3147=ORIENTED_EDGE('',*,*,#2305,.F.);
#3148=ORIENTED_EDGE('',*,*,#2309,.F.);
#3149=ORIENTED_EDGE('',*,*,#2312,.F.);
#3150=ORIENTED_EDGE('',*,*,#2315,.F.);
#3151=ORIENTED_EDGE('',*,*,#2318,.F.);
#3152=ORIENTED_EDGE('',*,*,#2321,.F.);
#3153=ORIENTED_EDGE('',*,*,#2324,.F.);
#3154=ORIENTED_EDGE('',*,*,#2327,.F.);
#3155=ORIENTED_EDGE('',*,*,#2330,.F.);
#3156=ORIENTED_EDGE('',*,*,#2333,.F.);
#3157=ORIENTED_EDGE('',*,*,#2336,.F.);
#3158=ORIENTED_EDGE('',*,*,#2339,.F.);
#3159=ORIENTED_EDGE('',*,*,#2342,.F.);
#3160=ORIENTED_EDGE('',*,*,#2345,.F.);
#3161=ORIENTED_EDGE('',*,*,#2348,.F.);
#3162=ORIENTED_EDGE('',*,*,#2351,.F.);
#3163=ORIENTED_EDGE('',*,*,#2354,.F.);
#3164=ORIENTED_EDGE('',*,*,#2364,.F.);
#3165=ORIENTED_EDGE('',*,*,#2359,.F.);
#3166=ORIENTED_EDGE('',*,*,#2366,.F.);
#3167=ORIENTED_EDGE('',*,*,#2301,.F.);
#3168=ORIENTED_EDGE('',*,*,#2367,.F.);
#3169=ORIENTED_EDGE('',*,*,#2299,.F.);
#3170=ORIENTED_EDGE('',*,*,#2296,.F.);
#3171=ORIENTED_EDGE('',*,*,#2293,.F.);
#3172=ORIENTED_EDGE('',*,*,#2290,.F.);
#3173=ORIENTED_EDGE('',*,*,#2287,.F.);
#3174=ORIENTED_EDGE('',*,*,#2284,.F.);
#3175=ORIENTED_EDGE('',*,*,#2281,.F.);
#3176=ORIENTED_EDGE('',*,*,#2278,.F.);
#3177=ORIENTED_EDGE('',*,*,#2275,.F.);
#3178=ORIENTED_EDGE('',*,*,#2272,.F.);
#3179=ORIENTED_EDGE('',*,*,#2269,.F.);
#3180=ORIENTED_EDGE('',*,*,#2266,.F.);
#3181=ORIENTED_EDGE('',*,*,#2263,.F.);
#3182=ORIENTED_EDGE('',*,*,#2260,.F.);
#3183=ORIENTED_EDGE('',*,*,#2257,.F.);
#3184=ORIENTED_EDGE('',*,*,#2254,.F.);
#3185=ORIENTED_EDGE('',*,*,#2358,.T.);
#3186=ORIENTED_EDGE('',*,*,#2368,.T.);
#3187=ORIENTED_EDGE('',*,*,#2369,.F.);
#3188=ORIENTED_EDGE('',*,*,#2370,.F.);
#3189=ORIENTED_EDGE('',*,*,#2366,.T.);
#3190=ORIENTED_EDGE('',*,*,#2362,.F.);
#3191=ORIENTED_EDGE('',*,*,#2252,.F.);
#3192=ORIENTED_EDGE('',*,*,#2256,.F.);
#3193=ORIENTED_EDGE('',*,*,#2259,.F.);
#3194=ORIENTED_EDGE('',*,*,#2262,.F.);
#3195=ORIENTED_EDGE('',*,*,#2265,.F.);
#3196=ORIENTED_EDGE('',*,*,#2268,.F.);
#3197=ORIENTED_EDGE('',*,*,#2271,.F.);
#3198=ORIENTED_EDGE('',*,*,#2274,.F.);
#3199=ORIENTED_EDGE('',*,*,#2277,.F.);
#3200=ORIENTED_EDGE('',*,*,#2280,.F.);
#3201=ORIENTED_EDGE('',*,*,#2283,.F.);
#3202=ORIENTED_EDGE('',*,*,#2286,.F.);
#3203=ORIENTED_EDGE('',*,*,#2289,.F.);
#3204=ORIENTED_EDGE('',*,*,#2292,.F.);
#3205=ORIENTED_EDGE('',*,*,#2295,.F.);
#3206=ORIENTED_EDGE('',*,*,#2298,.F.);
#3207=ORIENTED_EDGE('',*,*,#2371,.F.);
#3208=ORIENTED_EDGE('',*,*,#2303,.F.);
#3209=ORIENTED_EDGE('',*,*,#2368,.F.);
#3210=ORIENTED_EDGE('',*,*,#2357,.T.);
#3211=ORIENTED_EDGE('',*,*,#2365,.T.);
#3212=ORIENTED_EDGE('',*,*,#2355,.T.);
#3213=ORIENTED_EDGE('',*,*,#2352,.T.);
#3214=ORIENTED_EDGE('',*,*,#2349,.T.);
#3215=ORIENTED_EDGE('',*,*,#2346,.T.);
#3216=ORIENTED_EDGE('',*,*,#2343,.T.);
#3217=ORIENTED_EDGE('',*,*,#2340,.T.);
#3218=ORIENTED_EDGE('',*,*,#2337,.T.);
#3219=ORIENTED_EDGE('',*,*,#2334,.T.);
#3220=ORIENTED_EDGE('',*,*,#2331,.T.);
#3221=ORIENTED_EDGE('',*,*,#2328,.T.);
#3222=ORIENTED_EDGE('',*,*,#2325,.T.);
#3223=ORIENTED_EDGE('',*,*,#2322,.T.);
#3224=ORIENTED_EDGE('',*,*,#2319,.T.);
#3225=ORIENTED_EDGE('',*,*,#2316,.T.);
#3226=ORIENTED_EDGE('',*,*,#2313,.T.);
#3227=ORIENTED_EDGE('',*,*,#2310,.T.);
#3228=ORIENTED_EDGE('',*,*,#2307,.T.);
#3229=ORIENTED_EDGE('',*,*,#2372,.T.);
#3230=ORIENTED_EDGE('',*,*,#2369,.T.);
#3231=ORIENTED_EDGE('',*,*,#2302,.T.);
#3232=ORIENTED_EDGE('',*,*,#2370,.T.);
#3233=ORIENTED_EDGE('',*,*,#2372,.F.);
#3234=ORIENTED_EDGE('',*,*,#2300,.T.);
#3235=ORIENTED_EDGE('',*,*,#2371,.T.);
#3236=ORIENTED_EDGE('',*,*,#2297,.F.);
#3237=ORIENTED_EDGE('',*,*,#2367,.T.);
#3238=ORIENTED_EDGE('',*,*,#2360,.F.);
#3239=ORIENTED_EDGE('',*,*,#2253,.F.);
#3240=ORIENTED_EDGE('',*,*,#2361,.F.);
#3241=ORIENTED_EDGE('',*,*,#2373,.T.);
#3242=ORIENTED_EDGE('',*,*,#2374,.F.);
#3243=ORIENTED_EDGE('',*,*,#2373,.F.);
#3244=ORIENTED_EDGE('',*,*,#2375,.F.);
#3245=ORIENTED_EDGE('',*,*,#2376,.F.);
#3246=ORIENTED_EDGE('',*,*,#2377,.F.);
#3247=ORIENTED_EDGE('',*,*,#2378,.F.);
#3248=ORIENTED_EDGE('',*,*,#2379,.F.);
#3249=ORIENTED_EDGE('',*,*,#2378,.T.);
#3250=ORIENTED_EDGE('',*,*,#2380,.F.);
#3251=ORIENTED_EDGE('',*,*,#2381,.T.);
#3252=ORIENTED_EDGE('',*,*,#2382,.F.);
#3253=ORIENTED_EDGE('',*,*,#2381,.F.);
#3254=ORIENTED_EDGE('',*,*,#2383,.F.);
#3255=ORIENTED_EDGE('',*,*,#2384,.F.);
#3256=ORIENTED_EDGE('',*,*,#2385,.F.);
#3257=ORIENTED_EDGE('',*,*,#2384,.T.);
#3258=ORIENTED_EDGE('',*,*,#2386,.T.);
#3259=ORIENTED_EDGE('',*,*,#2376,.T.);
#3260=ORIENTED_EDGE('',*,*,#2386,.F.);
#3261=ORIENTED_EDGE('',*,*,#2383,.T.);
#3262=ORIENTED_EDGE('',*,*,#2380,.T.);
#3263=ORIENTED_EDGE('',*,*,#2377,.T.);
#3264=ORIENTED_EDGE('',*,*,#2387,.F.);
#3265=ORIENTED_EDGE('',*,*,#2388,.F.);
#3266=ORIENTED_EDGE('',*,*,#2389,.F.);
#3267=ORIENTED_EDGE('',*,*,#2390,.F.);
#3268=ORIENTED_EDGE('',*,*,#2391,.F.);
#3269=ORIENTED_EDGE('',*,*,#2390,.T.);
#3270=ORIENTED_EDGE('',*,*,#2392,.F.);
#3271=ORIENTED_EDGE('',*,*,#2393,.T.);
#3272=ORIENTED_EDGE('',*,*,#2394,.F.);
#3273=ORIENTED_EDGE('',*,*,#2393,.F.);
#3274=ORIENTED_EDGE('',*,*,#2395,.F.);
#3275=ORIENTED_EDGE('',*,*,#2396,.F.);
#3276=ORIENTED_EDGE('',*,*,#2397,.F.);
#3277=ORIENTED_EDGE('',*,*,#2396,.T.);
#3278=ORIENTED_EDGE('',*,*,#2398,.T.);
#3279=ORIENTED_EDGE('',*,*,#2388,.T.);
#3280=ORIENTED_EDGE('',*,*,#2398,.F.);
#3281=ORIENTED_EDGE('',*,*,#2395,.T.);
#3282=ORIENTED_EDGE('',*,*,#2392,.T.);
#3283=ORIENTED_EDGE('',*,*,#2389,.T.);
#3284=ORIENTED_EDGE('',*,*,#2399,.F.);
#3285=ORIENTED_EDGE('',*,*,#2400,.T.);
#3286=ORIENTED_EDGE('',*,*,#2401,.T.);
#3287=ORIENTED_EDGE('',*,*,#2402,.T.);
#3288=ORIENTED_EDGE('',*,*,#2400,.F.);
#3289=ORIENTED_EDGE('',*,*,#2402,.F.);
#3290=ORIENTED_EDGE('',*,*,#2403,.F.);
#3291=ORIENTED_EDGE('',*,*,#2401,.F.);
#3292=ORIENTED_EDGE('',*,*,#2403,.T.);
#3293=ORIENTED_EDGE('',*,*,#2404,.T.);
#3294=ORIENTED_EDGE('',*,*,#2405,.T.);
#3295=ORIENTED_EDGE('',*,*,#2404,.F.);
#3296=ORIENTED_EDGE('',*,*,#2382,.T.);
#3297=ORIENTED_EDGE('',*,*,#2385,.T.);
#3298=ORIENTED_EDGE('',*,*,#2375,.T.);
#3299=ORIENTED_EDGE('',*,*,#2379,.T.);
#3300=ORIENTED_EDGE('',*,*,#2394,.T.);
#3301=ORIENTED_EDGE('',*,*,#2397,.T.);
#3302=ORIENTED_EDGE('',*,*,#2387,.T.);
#3303=ORIENTED_EDGE('',*,*,#2391,.T.);
#3304=ORIENTED_EDGE('',*,*,#2405,.F.);
#3305=ORIENTED_EDGE('',*,*,#2406,.T.);
#3306=ORIENTED_EDGE('',*,*,#2407,.T.);
#3307=ORIENTED_EDGE('',*,*,#2408,.T.);
#3308=ORIENTED_EDGE('',*,*,#2406,.F.);
#3309=ORIENTED_EDGE('',*,*,#2408,.F.);
#3310=ORIENTED_EDGE('',*,*,#2409,.F.);
#3311=ORIENTED_EDGE('',*,*,#2407,.F.);
#3312=ORIENTED_EDGE('',*,*,#2409,.T.);
#3313=ORIENTED_EDGE('',*,*,#2410,.T.);
#3314=ORIENTED_EDGE('',*,*,#2411,.T.);
#3315=ORIENTED_EDGE('',*,*,#2410,.F.);
#3316=ORIENTED_EDGE('',*,*,#2412,.F.);
#3317=ORIENTED_EDGE('',*,*,#2411,.F.);
#3318=ORIENTED_EDGE('',*,*,#2413,.T.);
#3319=ORIENTED_EDGE('',*,*,#2412,.T.);
#3320=ORIENTED_EDGE('',*,*,#2413,.F.);
#3321=ORIENTED_EDGE('',*,*,#2414,.F.);
#3322=ORIENTED_EDGE('',*,*,#2415,.T.);
#3323=ORIENTED_EDGE('',*,*,#2399,.T.);
#3324=ORIENTED_EDGE('',*,*,#2415,.F.);
#3325=ORIENTED_EDGE('',*,*,#2416,.F.);
#3326=ORIENTED_EDGE('',*,*,#2417,.T.);
#3327=ORIENTED_EDGE('',*,*,#2414,.T.);
#3328=ORIENTED_EDGE('',*,*,#2417,.F.);
#3329=ORIENTED_EDGE('',*,*,#2416,.T.);
#3330=ORIENTED_EDGE('',*,*,#2374,.T.);
#3331=ORIENTED_EDGE('',*,*,#2418,.T.);
#3332=ORIENTED_EDGE('',*,*,#2419,.T.);
#3333=ORIENTED_EDGE('',*,*,#2420,.T.);
#3334=ORIENTED_EDGE('',*,*,#2421,.T.);
#3335=ORIENTED_EDGE('',*,*,#2422,.T.);
#3336=ORIENTED_EDGE('',*,*,#2423,.T.);
#3337=ORIENTED_EDGE('',*,*,#2420,.F.);
#3338=ORIENTED_EDGE('',*,*,#2424,.T.);
#3339=ORIENTED_EDGE('',*,*,#2418,.F.);
#3340=ORIENTED_EDGE('',*,*,#2425,.T.);
#3341=ORIENTED_EDGE('',*,*,#2424,.F.);
#3342=ORIENTED_EDGE('',*,*,#2426,.T.);
#3343=ORIENTED_EDGE('',*,*,#2427,.F.);
#3344=ORIENTED_EDGE('',*,*,#2428,.T.);
#3345=ORIENTED_EDGE('',*,*,#2425,.F.);
#3346=ORIENTED_EDGE('',*,*,#2429,.T.);
#3347=ORIENTED_EDGE('',*,*,#2430,.T.);
#3348=ORIENTED_EDGE('',*,*,#2431,.T.);
#3349=ORIENTED_EDGE('',*,*,#2421,.F.);
#3350=ORIENTED_EDGE('',*,*,#2432,.F.);
#3351=ORIENTED_EDGE('',*,*,#2433,.F.);
#3352=ORIENTED_EDGE('',*,*,#2429,.F.);
#3353=ORIENTED_EDGE('',*,*,#2434,.T.);
#3354=ORIENTED_EDGE('',*,*,#2435,.T.);
#3355=ORIENTED_EDGE('',*,*,#2436,.T.);
#3356=ORIENTED_EDGE('',*,*,#2437,.T.);
#3357=ORIENTED_EDGE('',*,*,#2434,.F.);
#3358=ORIENTED_EDGE('',*,*,#2438,.T.);
#3359=ORIENTED_EDGE('',*,*,#2439,.T.);
#3360=ORIENTED_EDGE('',*,*,#2427,.T.);
#3361=ORIENTED_EDGE('',*,*,#2440,.T.);
#3362=ORIENTED_EDGE('',*,*,#2436,.F.);
#3363=ORIENTED_EDGE('',*,*,#2422,.F.);
#3364=ORIENTED_EDGE('',*,*,#2441,.T.);
#3365=ORIENTED_EDGE('',*,*,#2439,.F.);
#3366=ORIENTED_EDGE('',*,*,#2442,.T.);
#3367=ORIENTED_EDGE('',*,*,#2438,.F.);
#3368=ORIENTED_EDGE('',*,*,#2443,.T.);
#3369=ORIENTED_EDGE('',*,*,#2444,.T.);
#3370=ORIENTED_EDGE('',*,*,#2445,.T.);
#3371=ORIENTED_EDGE('',*,*,#2446,.T.);
#3372=ORIENTED_EDGE('',*,*,#2437,.F.);
#3373=ORIENTED_EDGE('',*,*,#2447,.F.);
#3374=ORIENTED_EDGE('',*,*,#2448,.F.);
#3375=ORIENTED_EDGE('',*,*,#2449,.F.);
#3376=ORIENTED_EDGE('',*,*,#2450,.F.);
#3377=ORIENTED_EDGE('',*,*,#2449,.T.);
#3378=ORIENTED_EDGE('',*,*,#2451,.F.);
#3379=ORIENTED_EDGE('',*,*,#2443,.F.);
#3380=ORIENTED_EDGE('',*,*,#2440,.F.);
#3381=ORIENTED_EDGE('',*,*,#2452,.T.);
#3382=ORIENTED_EDGE('',*,*,#2453,.T.);
#3383=ORIENTED_EDGE('',*,*,#2454,.F.);
#3384=ORIENTED_EDGE('',*,*,#2447,.T.);
#3385=ORIENTED_EDGE('',*,*,#2426,.F.);
#3386=ORIENTED_EDGE('',*,*,#2431,.F.);
#3387=ORIENTED_EDGE('',*,*,#2455,.F.);
#3388=ORIENTED_EDGE('',*,*,#2456,.F.);
#3389=ORIENTED_EDGE('',*,*,#2452,.F.);
#3390=ORIENTED_EDGE('',*,*,#2457,.T.);
#3391=ORIENTED_EDGE('',*,*,#2458,.T.);
#3392=ORIENTED_EDGE('',*,*,#2459,.T.);
#3393=ORIENTED_EDGE('',*,*,#2457,.F.);
#3394=ORIENTED_EDGE('',*,*,#2450,.T.);
#3395=ORIENTED_EDGE('',*,*,#2460,.T.);
#3396=ORIENTED_EDGE('',*,*,#2461,.T.);
#3397=ORIENTED_EDGE('',*,*,#2458,.F.);
#3398=ORIENTED_EDGE('',*,*,#2459,.F.);
#3399=ORIENTED_EDGE('',*,*,#2461,.F.);
#3400=ORIENTED_EDGE('',*,*,#2462,.T.);
#3401=ORIENTED_EDGE('',*,*,#2463,.T.);
#3402=ORIENTED_EDGE('',*,*,#2464,.T.);
#3403=ORIENTED_EDGE('',*,*,#2465,.T.);
#3404=ORIENTED_EDGE('',*,*,#2464,.F.);
#3405=ORIENTED_EDGE('',*,*,#2465,.F.);
#3406=ORIENTED_EDGE('',*,*,#2466,.F.);
#3407=ORIENTED_EDGE('',*,*,#2467,.F.);
#3408=ORIENTED_EDGE('',*,*,#2468,.F.);
#3409=ORIENTED_EDGE('',*,*,#2469,.F.);
#3410=ORIENTED_EDGE('',*,*,#2470,.F.);
#3411=ORIENTED_EDGE('',*,*,#2471,.T.);
#3412=ORIENTED_EDGE('',*,*,#2462,.F.);
#3413=ORIENTED_EDGE('',*,*,#2463,.F.);
#3414=ORIENTED_EDGE('',*,*,#2471,.F.);
#3415=ORIENTED_EDGE('',*,*,#2469,.T.);
#3416=ORIENTED_EDGE('',*,*,#2472,.T.);
#3417=ORIENTED_EDGE('',*,*,#2473,.T.);
#3418=ORIENTED_EDGE('',*,*,#2474,.T.);
#3419=ORIENTED_EDGE('',*,*,#2475,.T.);
#3420=ORIENTED_EDGE('',*,*,#2476,.T.);
#3421=ORIENTED_EDGE('',*,*,#2466,.T.);
#3422=ORIENTED_EDGE('',*,*,#2474,.F.);
#3423=ORIENTED_EDGE('',*,*,#2476,.F.);
#3424=ORIENTED_EDGE('',*,*,#2477,.T.);
#3425=ORIENTED_EDGE('',*,*,#2478,.T.);
#3426=ORIENTED_EDGE('',*,*,#2478,.F.);
#3427=ORIENTED_EDGE('',*,*,#2479,.T.);
#3428=ORIENTED_EDGE('',*,*,#2480,.T.);
#3429=ORIENTED_EDGE('',*,*,#2467,.T.);
#3430=ORIENTED_EDGE('',*,*,#2477,.F.);
#3431=ORIENTED_EDGE('',*,*,#2481,.T.);
#3432=ORIENTED_EDGE('',*,*,#2482,.F.);
#3433=ORIENTED_EDGE('',*,*,#2483,.T.);
#3434=ORIENTED_EDGE('',*,*,#2475,.F.);
#3435=ORIENTED_EDGE('',*,*,#2484,.F.);
#3436=ORIENTED_EDGE('',*,*,#2485,.F.);
#3437=ORIENTED_EDGE('',*,*,#2481,.F.);
#3438=ORIENTED_EDGE('',*,*,#2473,.F.);
#3439=ORIENTED_EDGE('',*,*,#2486,.T.);
#3440=ORIENTED_EDGE('',*,*,#2487,.F.);
#3441=ORIENTED_EDGE('',*,*,#2484,.T.);
#3442=ORIENTED_EDGE('',*,*,#2487,.T.);
#3443=ORIENTED_EDGE('',*,*,#2488,.T.);
#3444=ORIENTED_EDGE('',*,*,#2489,.T.);
#3445=ORIENTED_EDGE('',*,*,#2490,.T.);
#3446=ORIENTED_EDGE('',*,*,#2491,.T.);
#3447=ORIENTED_EDGE('',*,*,#2492,.T.);
#3448=ORIENTED_EDGE('',*,*,#2482,.T.);
#3449=ORIENTED_EDGE('',*,*,#2493,.T.);
#3450=ORIENTED_EDGE('',*,*,#2491,.F.);
#3451=ORIENTED_EDGE('',*,*,#2485,.T.);
#3452=ORIENTED_EDGE('',*,*,#2490,.F.);
#3453=ORIENTED_EDGE('',*,*,#2492,.F.);
#3454=ORIENTED_EDGE('',*,*,#2494,.T.);
#3455=ORIENTED_EDGE('',*,*,#2495,.T.);
#3456=ORIENTED_EDGE('',*,*,#2496,.T.);
#3457=ORIENTED_EDGE('',*,*,#2497,.T.);
#3458=ORIENTED_EDGE('',*,*,#2498,.T.);
#3459=ORIENTED_EDGE('',*,*,#2499,.T.);
#3460=ORIENTED_EDGE('',*,*,#2500,.T.);
#3461=ORIENTED_EDGE('',*,*,#2498,.F.);
#3462=ORIENTED_EDGE('',*,*,#2497,.F.);
#3463=ORIENTED_EDGE('',*,*,#2501,.F.);
#3464=ORIENTED_EDGE('',*,*,#2494,.F.);
#3465=ORIENTED_EDGE('',*,*,#2493,.F.);
#3466=ORIENTED_EDGE('',*,*,#2489,.F.);
#3467=ORIENTED_EDGE('',*,*,#2500,.F.);
#3468=ORIENTED_EDGE('',*,*,#2502,.T.);
#3469=ORIENTED_EDGE('',*,*,#2503,.T.);
#3470=ORIENTED_EDGE('',*,*,#2504,.T.);
#3471=ORIENTED_EDGE('',*,*,#2502,.F.);
#3472=ORIENTED_EDGE('',*,*,#2499,.F.);
#3473=ORIENTED_EDGE('',*,*,#2505,.F.);
#3474=ORIENTED_EDGE('',*,*,#2506,.F.);
#3475=ORIENTED_EDGE('',*,*,#2480,.F.);
#3476=ORIENTED_EDGE('',*,*,#2468,.T.);
#3477=ORIENTED_EDGE('',*,*,#2506,.T.);
#3478=ORIENTED_EDGE('',*,*,#2507,.T.);
#3479=ORIENTED_EDGE('',*,*,#2472,.F.);
#3480=ORIENTED_EDGE('',*,*,#2508,.T.);
#3481=ORIENTED_EDGE('',*,*,#2509,.T.);
#3482=ORIENTED_EDGE('',*,*,#2505,.T.);
#3483=ORIENTED_EDGE('',*,*,#2510,.T.);
#3484=ORIENTED_EDGE('',*,*,#2495,.F.);
#3485=ORIENTED_EDGE('',*,*,#2511,.T.);
#3486=ORIENTED_EDGE('',*,*,#2508,.F.);
#3487=ORIENTED_EDGE('',*,*,#2507,.F.);
#3488=ORIENTED_EDGE('',*,*,#2509,.F.);
#3489=ORIENTED_EDGE('',*,*,#2512,.F.);
#3490=ORIENTED_EDGE('',*,*,#2486,.F.);
#3491=ORIENTED_EDGE('',*,*,#2511,.F.);
#3492=ORIENTED_EDGE('',*,*,#2501,.T.);
#3493=ORIENTED_EDGE('',*,*,#2488,.F.);
#3494=ORIENTED_EDGE('',*,*,#2512,.T.);
#3495=ORIENTED_EDGE('',*,*,#2496,.F.);
#3496=ORIENTED_EDGE('',*,*,#2510,.F.);
#3497=ORIENTED_EDGE('',*,*,#2479,.F.);
#3498=ORIENTED_EDGE('',*,*,#2483,.F.);
#3499=ORIENTED_EDGE('',*,*,#2513,.T.);
#3500=ORIENTED_EDGE('',*,*,#2514,.T.);
#3501=ORIENTED_EDGE('',*,*,#2515,.T.);
#3502=ORIENTED_EDGE('',*,*,#2433,.T.);
#3503=ORIENTED_EDGE('',*,*,#2423,.F.);
#3504=ORIENTED_EDGE('',*,*,#2516,.T.);
#3505=ORIENTED_EDGE('',*,*,#2517,.T.);
#3506=ORIENTED_EDGE('',*,*,#2432,.T.);
#3507=ORIENTED_EDGE('',*,*,#2517,.F.);
#3508=ORIENTED_EDGE('',*,*,#2518,.T.);
#3509=ORIENTED_EDGE('',*,*,#2513,.F.);
#3510=ORIENTED_EDGE('',*,*,#2515,.F.);
#3511=ORIENTED_EDGE('',*,*,#2519,.T.);
#3512=ORIENTED_EDGE('',*,*,#2430,.F.);
#3513=ORIENTED_EDGE('',*,*,#2519,.F.);
#3514=ORIENTED_EDGE('',*,*,#2520,.T.);
#3515=ORIENTED_EDGE('',*,*,#2521,.F.);
#3516=ORIENTED_EDGE('',*,*,#2522,.T.);
#3517=ORIENTED_EDGE('',*,*,#2455,.T.);
#3518=ORIENTED_EDGE('',*,*,#2514,.F.);
#3519=ORIENTED_EDGE('',*,*,#2523,.F.);
#3520=ORIENTED_EDGE('',*,*,#2524,.F.);
#3521=ORIENTED_EDGE('',*,*,#2525,.T.);
#3522=ORIENTED_EDGE('',*,*,#2503,.F.);
#3523=ORIENTED_EDGE('',*,*,#2504,.F.);
#3524=ORIENTED_EDGE('',*,*,#2525,.F.);
#3525=ORIENTED_EDGE('',*,*,#2526,.F.);
#3526=ORIENTED_EDGE('',*,*,#2520,.F.);
#3527=ORIENTED_EDGE('',*,*,#2518,.F.);
#3528=ORIENTED_EDGE('',*,*,#2527,.T.);
#3529=ORIENTED_EDGE('',*,*,#2528,.T.);
#3530=ORIENTED_EDGE('',*,*,#2529,.T.);
#3531=ORIENTED_EDGE('',*,*,#2523,.T.);
#3532=ORIENTED_EDGE('',*,*,#2442,.F.);
#3533=ORIENTED_EDGE('',*,*,#2446,.F.);
#3534=ORIENTED_EDGE('',*,*,#2530,.F.);
#3535=ORIENTED_EDGE('',*,*,#2527,.F.);
#3536=ORIENTED_EDGE('',*,*,#2516,.F.);
#3537=ORIENTED_EDGE('',*,*,#2451,.T.);
#3538=ORIENTED_EDGE('',*,*,#2448,.T.);
#3539=ORIENTED_EDGE('',*,*,#2454,.T.);
#3540=ORIENTED_EDGE('',*,*,#2531,.T.);
#3541=ORIENTED_EDGE('',*,*,#2532,.T.);
#3542=ORIENTED_EDGE('',*,*,#2533,.F.);
#3543=ORIENTED_EDGE('',*,*,#2444,.F.);
#3544=ORIENTED_EDGE('',*,*,#2532,.F.);
#3545=ORIENTED_EDGE('',*,*,#2531,.F.);
#3546=ORIENTED_EDGE('',*,*,#2453,.F.);
#3547=ORIENTED_EDGE('',*,*,#2456,.T.);
#3548=ORIENTED_EDGE('',*,*,#2522,.F.);
#3549=ORIENTED_EDGE('',*,*,#2534,.F.);
#3550=ORIENTED_EDGE('',*,*,#2535,.F.);
#3551=ORIENTED_EDGE('',*,*,#2536,.T.);
#3552=ORIENTED_EDGE('',*,*,#2528,.F.);
#3553=ORIENTED_EDGE('',*,*,#2530,.T.);
#3554=ORIENTED_EDGE('',*,*,#2445,.F.);
#3555=ORIENTED_EDGE('',*,*,#2533,.T.);
#3556=ORIENTED_EDGE('',*,*,#2535,.T.);
#3557=ORIENTED_EDGE('',*,*,#2534,.T.);
#3558=ORIENTED_EDGE('',*,*,#2521,.T.);
#3559=ORIENTED_EDGE('',*,*,#2526,.T.);
#3560=ORIENTED_EDGE('',*,*,#2524,.T.);
#3561=ORIENTED_EDGE('',*,*,#2529,.F.);
#3562=ORIENTED_EDGE('',*,*,#2536,.F.);
#3563=ORIENTED_EDGE('',*,*,#2460,.F.);
#3564=ORIENTED_EDGE('',*,*,#2470,.T.);
#3565=ORIENTED_EDGE('',*,*,#2419,.F.);
#3566=ORIENTED_EDGE('',*,*,#2428,.F.);
#3567=ORIENTED_EDGE('',*,*,#2435,.F.);
#3568=ORIENTED_EDGE('',*,*,#2441,.F.);
#3569=ORIENTED_EDGE('',*,*,#2537,.T.);
#3570=ORIENTED_EDGE('',*,*,#2538,.T.);
#3571=ORIENTED_EDGE('',*,*,#2539,.T.);
#3572=ORIENTED_EDGE('',*,*,#2540,.T.);
#3573=ORIENTED_EDGE('',*,*,#2539,.F.);
#3574=ORIENTED_EDGE('',*,*,#2541,.F.);
#3575=ORIENTED_EDGE('',*,*,#2542,.F.);
#3576=ORIENTED_EDGE('',*,*,#2543,.T.);
#3577=ORIENTED_EDGE('',*,*,#2537,.F.);
#3578=ORIENTED_EDGE('',*,*,#2538,.F.);
#3579=ORIENTED_EDGE('',*,*,#2543,.F.);
#3580=ORIENTED_EDGE('',*,*,#2540,.F.);
#3581=ORIENTED_EDGE('',*,*,#2544,.T.);
#3582=ORIENTED_EDGE('',*,*,#2545,.T.);
#3583=ORIENTED_EDGE('',*,*,#2546,.T.);
#3584=ORIENTED_EDGE('',*,*,#2541,.T.);
#3585=ORIENTED_EDGE('',*,*,#2542,.T.);
#3586=ORIENTED_EDGE('',*,*,#2546,.F.);
#3587=ORIENTED_EDGE('',*,*,#2545,.F.);
#3588=ORIENTED_EDGE('',*,*,#2547,.T.);
#3589=ORIENTED_EDGE('',*,*,#2548,.F.);
#3590=ORIENTED_EDGE('',*,*,#2549,.F.);
#3591=ORIENTED_EDGE('',*,*,#2550,.F.);
#3592=ORIENTED_EDGE('',*,*,#2551,.T.);
#3593=ORIENTED_EDGE('',*,*,#2552,.F.);
#3594=ORIENTED_EDGE('',*,*,#2553,.T.);
#3595=ORIENTED_EDGE('',*,*,#2554,.F.);
#3596=ORIENTED_EDGE('',*,*,#2555,.F.);
#3597=ORIENTED_EDGE('',*,*,#2556,.F.);
#3598=ORIENTED_EDGE('',*,*,#2551,.F.);
#3599=ORIENTED_EDGE('',*,*,#2557,.F.);
#3600=ORIENTED_EDGE('',*,*,#2558,.F.);
#3601=ORIENTED_EDGE('',*,*,#2559,.F.);
#3602=ORIENTED_EDGE('',*,*,#2553,.F.);
#3603=ORIENTED_EDGE('',*,*,#2560,.F.);
#3604=ORIENTED_EDGE('',*,*,#2561,.F.);
#3605=ORIENTED_EDGE('',*,*,#2549,.T.);
#3606=ORIENTED_EDGE('',*,*,#2562,.F.);
#3607=ORIENTED_EDGE('',*,*,#2555,.T.);
#3608=ORIENTED_EDGE('',*,*,#2563,.F.);
#3609=ORIENTED_EDGE('',*,*,#2563,.T.);
#3610=ORIENTED_EDGE('',*,*,#2554,.T.);
#3611=ORIENTED_EDGE('',*,*,#2559,.T.);
#3612=ORIENTED_EDGE('',*,*,#2564,.F.);
#3613=ORIENTED_EDGE('',*,*,#2565,.F.);
#3614=ORIENTED_EDGE('',*,*,#2566,.F.);
#3615=ORIENTED_EDGE('',*,*,#2567,.F.);
#3616=ORIENTED_EDGE('',*,*,#2568,.F.);
#3617=ORIENTED_EDGE('',*,*,#2569,.F.);
#3618=ORIENTED_EDGE('',*,*,#2570,.T.);
#3619=ORIENTED_EDGE('',*,*,#2571,.F.);
#3620=ORIENTED_EDGE('',*,*,#2572,.T.);
#3621=ORIENTED_EDGE('',*,*,#2573,.F.);
#3622=ORIENTED_EDGE('',*,*,#2574,.F.);
#3623=ORIENTED_EDGE('',*,*,#2575,.F.);
#3624=ORIENTED_EDGE('',*,*,#2576,.T.);
#3625=ORIENTED_EDGE('',*,*,#2573,.T.);
#3626=ORIENTED_EDGE('',*,*,#2577,.T.);
#3627=ORIENTED_EDGE('',*,*,#2578,.T.);
#3628=ORIENTED_EDGE('',*,*,#2579,.T.);
#3629=ORIENTED_EDGE('',*,*,#2580,.T.);
#3630=ORIENTED_EDGE('',*,*,#2581,.T.);
#3631=ORIENTED_EDGE('',*,*,#2582,.T.);
#3632=ORIENTED_EDGE('',*,*,#2580,.F.);
#3633=ORIENTED_EDGE('',*,*,#2582,.F.);
#3634=ORIENTED_EDGE('',*,*,#2583,.T.);
#3635=ORIENTED_EDGE('',*,*,#2547,.F.);
#3636=ORIENTED_EDGE('',*,*,#2583,.F.);
#3637=ORIENTED_EDGE('',*,*,#2581,.F.);
#3638=ORIENTED_EDGE('',*,*,#2584,.F.);
#3639=ORIENTED_EDGE('',*,*,#2585,.T.);
#3640=ORIENTED_EDGE('',*,*,#2578,.F.);
#3641=ORIENTED_EDGE('',*,*,#2579,.F.);
#3642=ORIENTED_EDGE('',*,*,#2585,.F.);
#3643=ORIENTED_EDGE('',*,*,#2586,.F.);
#3644=ORIENTED_EDGE('',*,*,#2544,.F.);
#3645=ORIENTED_EDGE('',*,*,#2587,.T.);
#3646=ORIENTED_EDGE('',*,*,#2588,.T.);
#3647=ORIENTED_EDGE('',*,*,#2589,.T.);
#3648=ORIENTED_EDGE('',*,*,#2587,.F.);
#3649=ORIENTED_EDGE('',*,*,#2589,.F.);
#3650=ORIENTED_EDGE('',*,*,#2590,.T.);
#3651=ORIENTED_EDGE('',*,*,#2591,.F.);
#3652=ORIENTED_EDGE('',*,*,#2592,.F.);
#3653=ORIENTED_EDGE('',*,*,#2577,.F.);
#3654=ORIENTED_EDGE('',*,*,#2572,.F.);
#3655=ORIENTED_EDGE('',*,*,#2593,.F.);
#3656=ORIENTED_EDGE('',*,*,#2590,.F.);
#3657=ORIENTED_EDGE('',*,*,#2588,.F.);
#3658=ORIENTED_EDGE('',*,*,#2594,.T.);
#3659=ORIENTED_EDGE('',*,*,#2591,.T.);
#3660=ORIENTED_EDGE('',*,*,#2593,.T.);
#3661=ORIENTED_EDGE('',*,*,#2571,.T.);
#3662=ORIENTED_EDGE('',*,*,#2595,.T.);
#3663=ORIENTED_EDGE('',*,*,#2596,.T.);
#3664=ORIENTED_EDGE('',*,*,#2597,.T.);
#3665=ORIENTED_EDGE('',*,*,#2598,.T.);
#3666=ORIENTED_EDGE('',*,*,#2599,.T.);
#3667=ORIENTED_EDGE('',*,*,#2597,.F.);
#3668=ORIENTED_EDGE('',*,*,#2600,.F.);
#3669=ORIENTED_EDGE('',*,*,#2601,.F.);
#3670=ORIENTED_EDGE('',*,*,#2602,.F.);
#3671=ORIENTED_EDGE('',*,*,#2596,.F.);
#3672=ORIENTED_EDGE('',*,*,#2603,.F.);
#3673=ORIENTED_EDGE('',*,*,#2569,.T.);
#3674=ORIENTED_EDGE('',*,*,#2604,.T.);
#3675=ORIENTED_EDGE('',*,*,#2600,.T.);
#3676=ORIENTED_EDGE('',*,*,#2595,.F.);
#3677=ORIENTED_EDGE('',*,*,#2570,.F.);
#3678=ORIENTED_EDGE('',*,*,#2603,.T.);
#3679=ORIENTED_EDGE('',*,*,#2599,.F.);
#3680=ORIENTED_EDGE('',*,*,#2605,.F.);
#3681=ORIENTED_EDGE('',*,*,#2606,.F.);
#3682=ORIENTED_EDGE('',*,*,#2598,.F.);
#3683=ORIENTED_EDGE('',*,*,#2602,.T.);
#3684=ORIENTED_EDGE('',*,*,#2607,.T.);
#3685=ORIENTED_EDGE('',*,*,#2608,.T.);
#3686=ORIENTED_EDGE('',*,*,#2605,.T.);
#3687=ORIENTED_EDGE('',*,*,#2609,.T.);
#3688=ORIENTED_EDGE('',*,*,#2610,.T.);
#3689=ORIENTED_EDGE('',*,*,#2611,.T.);
#3690=ORIENTED_EDGE('',*,*,#2601,.T.);
#3691=ORIENTED_EDGE('',*,*,#2611,.F.);
#3692=ORIENTED_EDGE('',*,*,#2612,.T.);
#3693=ORIENTED_EDGE('',*,*,#2607,.F.);
#3694=ORIENTED_EDGE('',*,*,#2604,.F.);
#3695=ORIENTED_EDGE('',*,*,#2613,.T.);
#3696=ORIENTED_EDGE('',*,*,#2609,.F.);
#3697=ORIENTED_EDGE('',*,*,#2561,.T.);
#3698=ORIENTED_EDGE('',*,*,#2614,.F.);
#3699=ORIENTED_EDGE('',*,*,#2575,.T.);
#3700=ORIENTED_EDGE('',*,*,#2592,.T.);
#3701=ORIENTED_EDGE('',*,*,#2594,.F.);
#3702=ORIENTED_EDGE('',*,*,#2606,.T.);
#3703=ORIENTED_EDGE('',*,*,#2608,.F.);
#3704=ORIENTED_EDGE('',*,*,#2615,.F.);
#3705=ORIENTED_EDGE('',*,*,#2616,.F.);
#3706=ORIENTED_EDGE('',*,*,#2617,.F.);
#3707=ORIENTED_EDGE('',*,*,#2618,.F.);
#3708=ORIENTED_EDGE('',*,*,#2619,.F.);
#3709=ORIENTED_EDGE('',*,*,#2557,.T.);
#3710=ORIENTED_EDGE('',*,*,#2550,.T.);
#3711=ORIENTED_EDGE('',*,*,#2612,.F.);
#3712=ORIENTED_EDGE('',*,*,#2620,.T.);
#3713=ORIENTED_EDGE('',*,*,#2621,.T.);
#3714=ORIENTED_EDGE('',*,*,#2615,.T.);
#3715=ORIENTED_EDGE('',*,*,#2610,.F.);
#3716=ORIENTED_EDGE('',*,*,#2622,.F.);
#3717=ORIENTED_EDGE('',*,*,#2623,.F.);
#3718=ORIENTED_EDGE('',*,*,#2620,.F.);
#3719=ORIENTED_EDGE('',*,*,#2613,.F.);
#3720=ORIENTED_EDGE('',*,*,#2568,.T.);
#3721=ORIENTED_EDGE('',*,*,#2624,.T.);
#3722=ORIENTED_EDGE('',*,*,#2622,.T.);
#3723=ORIENTED_EDGE('',*,*,#2625,.T.);
#3724=ORIENTED_EDGE('',*,*,#2626,.T.);
#3725=ORIENTED_EDGE('',*,*,#2586,.T.);
#3726=ORIENTED_EDGE('',*,*,#2584,.T.);
#3727=ORIENTED_EDGE('',*,*,#2626,.F.);
#3728=ORIENTED_EDGE('',*,*,#2625,.F.);
#3729=ORIENTED_EDGE('',*,*,#2627,.F.);
#3730=ORIENTED_EDGE('',*,*,#2628,.T.);
#3731=ORIENTED_EDGE('',*,*,#2629,.T.);
#3732=ORIENTED_EDGE('',*,*,#2630,.T.);
#3733=ORIENTED_EDGE('',*,*,#2627,.T.);
#3734=ORIENTED_EDGE('',*,*,#2630,.F.);
#3735=ORIENTED_EDGE('',*,*,#2628,.F.);
#3736=ORIENTED_EDGE('',*,*,#2629,.F.);
#3737=ORIENTED_EDGE('',*,*,#2631,.T.);
#3738=ORIENTED_EDGE('',*,*,#2632,.F.);
#3739=ORIENTED_EDGE('',*,*,#2633,.F.);
#3740=ORIENTED_EDGE('',*,*,#2634,.F.);
#3741=ORIENTED_EDGE('',*,*,#2635,.F.);
#3742=ORIENTED_EDGE('',*,*,#2636,.F.);
#3743=ORIENTED_EDGE('',*,*,#2631,.F.);
#3744=ORIENTED_EDGE('',*,*,#2562,.T.);
#3745=ORIENTED_EDGE('',*,*,#2574,.T.);
#3746=ORIENTED_EDGE('',*,*,#2576,.F.);
#3747=ORIENTED_EDGE('',*,*,#2614,.T.);
#3748=ORIENTED_EDGE('',*,*,#2560,.T.);
#3749=ORIENTED_EDGE('',*,*,#2548,.T.);
#3750=ORIENTED_EDGE('',*,*,#2556,.T.);
#3751=ORIENTED_EDGE('',*,*,#2619,.T.);
#3752=ORIENTED_EDGE('',*,*,#2637,.T.);
#3753=ORIENTED_EDGE('',*,*,#2564,.T.);
#3754=ORIENTED_EDGE('',*,*,#2558,.T.);
#3755=ORIENTED_EDGE('',*,*,#2552,.T.);
#3756=ORIENTED_EDGE('',*,*,#2638,.F.);
#3757=ORIENTED_EDGE('',*,*,#2621,.F.);
#3758=ORIENTED_EDGE('',*,*,#2639,.F.);
#3759=ORIENTED_EDGE('',*,*,#2640,.F.);
#3760=ORIENTED_EDGE('',*,*,#2641,.F.);
#3761=ORIENTED_EDGE('',*,*,#2624,.F.);
#3762=ORIENTED_EDGE('',*,*,#2639,.T.);
#3763=ORIENTED_EDGE('',*,*,#2623,.T.);
#3764=ORIENTED_EDGE('',*,*,#2641,.T.);
#3765=ORIENTED_EDGE('',*,*,#2632,.T.);
#3766=ORIENTED_EDGE('',*,*,#2636,.T.);
#3767=ORIENTED_EDGE('',*,*,#2616,.T.);
#3768=ORIENTED_EDGE('',*,*,#2638,.T.);
#3769=ORIENTED_EDGE('',*,*,#2635,.T.);
#3770=ORIENTED_EDGE('',*,*,#2642,.T.);
#3771=ORIENTED_EDGE('',*,*,#2634,.T.);
#3772=ORIENTED_EDGE('',*,*,#2643,.T.);
#3773=ORIENTED_EDGE('',*,*,#2566,.T.);
#3774=ORIENTED_EDGE('',*,*,#2644,.T.);
#3775=ORIENTED_EDGE('',*,*,#2617,.T.);
#3776=ORIENTED_EDGE('',*,*,#2642,.F.);
#3777=ORIENTED_EDGE('',*,*,#2633,.T.);
#3778=ORIENTED_EDGE('',*,*,#2640,.T.);
#3779=ORIENTED_EDGE('',*,*,#2567,.T.);
#3780=ORIENTED_EDGE('',*,*,#2643,.F.);
#3781=ORIENTED_EDGE('',*,*,#2644,.F.);
#3782=ORIENTED_EDGE('',*,*,#2565,.T.);
#3783=ORIENTED_EDGE('',*,*,#2637,.F.);
#3784=ORIENTED_EDGE('',*,*,#2618,.T.);
#3785=ORIENTED_EDGE('',*,*,#2645,.T.);
#3786=ORIENTED_EDGE('',*,*,#2646,.T.);
#3787=ORIENTED_EDGE('',*,*,#2647,.T.);
#3788=ORIENTED_EDGE('',*,*,#2648,.T.);
#3789=ORIENTED_EDGE('',*,*,#2646,.F.);
#3790=ORIENTED_EDGE('',*,*,#2648,.F.);
#3791=ORIENTED_EDGE('',*,*,#2649,.T.);
#3792=ORIENTED_EDGE('',*,*,#2650,.F.);
#3793=ORIENTED_EDGE('',*,*,#2651,.F.);
#3794=ORIENTED_EDGE('',*,*,#2649,.F.);
#3795=ORIENTED_EDGE('',*,*,#2647,.F.);
#3796=ORIENTED_EDGE('',*,*,#2645,.F.);
#3797=ORIENTED_EDGE('',*,*,#2652,.F.);
#3798=ORIENTED_EDGE('',*,*,#2650,.T.);
#3799=ORIENTED_EDGE('',*,*,#2651,.T.);
#3800=ORIENTED_EDGE('',*,*,#2653,.T.);
#3801=ORIENTED_EDGE('',*,*,#2654,.T.);
#3802=ORIENTED_EDGE('',*,*,#2655,.T.);
#3803=ORIENTED_EDGE('',*,*,#2653,.F.);
#3804=ORIENTED_EDGE('',*,*,#2655,.F.);
#3805=ORIENTED_EDGE('',*,*,#2656,.T.);
#3806=ORIENTED_EDGE('',*,*,#2657,.F.);
#3807=ORIENTED_EDGE('',*,*,#2658,.F.);
#3808=ORIENTED_EDGE('',*,*,#2656,.F.);
#3809=ORIENTED_EDGE('',*,*,#2654,.F.);
#3810=ORIENTED_EDGE('',*,*,#2657,.T.);
#3811=ORIENTED_EDGE('',*,*,#2658,.T.);
#3812=ORIENTED_EDGE('',*,*,#2659,.T.);
#3813=ORIENTED_EDGE('',*,*,#2660,.T.);
#3814=ORIENTED_EDGE('',*,*,#2659,.F.);
#3815=ORIENTED_EDGE('',*,*,#2660,.F.);
#3816=ORIENTED_EDGE('',*,*,#2661,.F.);
#3817=ORIENTED_EDGE('',*,*,#2661,.T.);
#3818=ORIENTED_EDGE('',*,*,#2662,.T.);
#3819=ORIENTED_EDGE('',*,*,#2663,.T.);
#3820=ORIENTED_EDGE('',*,*,#2664,.T.);
#3821=ORIENTED_EDGE('',*,*,#2662,.F.);
#3822=ORIENTED_EDGE('',*,*,#2665,.F.);
#3823=ORIENTED_EDGE('',*,*,#2666,.F.);
#3824=ORIENTED_EDGE('',*,*,#2667,.T.);
#3825=ORIENTED_EDGE('',*,*,#2663,.F.);
#3826=ORIENTED_EDGE('',*,*,#2664,.F.);
#3827=ORIENTED_EDGE('',*,*,#2667,.F.);
#3828=ORIENTED_EDGE('',*,*,#2665,.T.);
#3829=ORIENTED_EDGE('',*,*,#2666,.T.);
#3830=ORIENTED_EDGE('',*,*,#2668,.T.);
#3831=ORIENTED_EDGE('',*,*,#2652,.T.);
#3832=ORIENTED_EDGE('',*,*,#2668,.F.);
#3833=ORIENTED_EDGE('',*,*,#2669,.F.);
#3834=ORIENTED_EDGE('',*,*,#2670,.T.);
#3835=ORIENTED_EDGE('',*,*,#2671,.T.);
#3836=ORIENTED_EDGE('',*,*,#2670,.F.);
#3837=ORIENTED_EDGE('',*,*,#2669,.T.);
#3838=ORIENTED_EDGE('',*,*,#2672,.F.);
#3839=ORIENTED_EDGE('',*,*,#2672,.T.);
#3840=ORIENTED_EDGE('',*,*,#2673,.T.);
#3841=ORIENTED_EDGE('',*,*,#2674,.F.);
#3842=ORIENTED_EDGE('',*,*,#2673,.F.);
#3843=ORIENTED_EDGE('',*,*,#2674,.T.);
#3844=ORIENTED_EDGE('',*,*,#2675,.T.);
#3845=ORIENTED_EDGE('',*,*,#2676,.F.);
#3846=ORIENTED_EDGE('',*,*,#2675,.F.);
#3847=ORIENTED_EDGE('',*,*,#2676,.T.);
#3848=ORIENTED_EDGE('',*,*,#2677,.T.);
#3849=ORIENTED_EDGE('',*,*,#2678,.F.);
#3850=ORIENTED_EDGE('',*,*,#2677,.F.);
#3851=ORIENTED_EDGE('',*,*,#2671,.F.);
#3852=ORIENTED_EDGE('',*,*,#2678,.T.);
#3853=ORIENTED_EDGE('',*,*,#2679,.F.);
#3854=ORIENTED_EDGE('',*,*,#2680,.T.);
#3855=ORIENTED_EDGE('',*,*,#2681,.T.);
#3856=ORIENTED_EDGE('',*,*,#2680,.F.);
#3857=ORIENTED_EDGE('',*,*,#2682,.F.);
#3858=ORIENTED_EDGE('',*,*,#2683,.T.);
#3859=ORIENTED_EDGE('',*,*,#2679,.T.);
#3860=ORIENTED_EDGE('',*,*,#2683,.F.);
#3861=ORIENTED_EDGE('',*,*,#2684,.F.);
#3862=ORIENTED_EDGE('',*,*,#2685,.T.);
#3863=ORIENTED_EDGE('',*,*,#2682,.T.);
#3864=ORIENTED_EDGE('',*,*,#2685,.F.);
#3865=ORIENTED_EDGE('',*,*,#2684,.T.);
#3866=ORIENTED_EDGE('',*,*,#2686,.F.);
#3867=ORIENTED_EDGE('',*,*,#2686,.T.);
#3868=ORIENTED_EDGE('',*,*,#2687,.T.);
#3869=ORIENTED_EDGE('',*,*,#2688,.F.);
#3870=ORIENTED_EDGE('',*,*,#2687,.F.);
#3871=ORIENTED_EDGE('',*,*,#2681,.F.);
#3872=ORIENTED_EDGE('',*,*,#2688,.T.);
#3873=ORIENTED_EDGE('',*,*,#2689,.F.);
#3874=ORIENTED_EDGE('',*,*,#2690,.T.);
#3875=ORIENTED_EDGE('',*,*,#2691,.F.);
#3876=ORIENTED_EDGE('',*,*,#2690,.F.);
#3877=ORIENTED_EDGE('',*,*,#2692,.F.);
#3878=ORIENTED_EDGE('',*,*,#2693,.T.);
#3879=ORIENTED_EDGE('',*,*,#2694,.F.);
#3880=ORIENTED_EDGE('',*,*,#2693,.F.);
#3881=ORIENTED_EDGE('',*,*,#2695,.T.);
#3882=ORIENTED_EDGE('',*,*,#2696,.T.);
#3883=ORIENTED_EDGE('',*,*,#2697,.T.);
#3884=ORIENTED_EDGE('',*,*,#2698,.T.);
#3885=ORIENTED_EDGE('',*,*,#2699,.T.);
#3886=ORIENTED_EDGE('',*,*,#2700,.T.);
#3887=ORIENTED_EDGE('',*,*,#2701,.T.);
#3888=ORIENTED_EDGE('',*,*,#2702,.F.);
#3889=ORIENTED_EDGE('',*,*,#2694,.T.);
#3890=ORIENTED_EDGE('',*,*,#2691,.T.);
#3891=ORIENTED_EDGE('',*,*,#2701,.F.);
#3892=ORIENTED_EDGE('',*,*,#2703,.F.);
#3893=ORIENTED_EDGE('',*,*,#2704,.F.);
#3894=ORIENTED_EDGE('',*,*,#2705,.F.);
#3895=ORIENTED_EDGE('',*,*,#2706,.F.);
#3896=ORIENTED_EDGE('',*,*,#2703,.T.);
#3897=ORIENTED_EDGE('',*,*,#2700,.F.);
#3898=ORIENTED_EDGE('',*,*,#2707,.F.);
#3899=ORIENTED_EDGE('',*,*,#2708,.F.);
#3900=ORIENTED_EDGE('',*,*,#2709,.F.);
#3901=ORIENTED_EDGE('',*,*,#2707,.T.);
#3902=ORIENTED_EDGE('',*,*,#2699,.F.);
#3903=ORIENTED_EDGE('',*,*,#2710,.T.);
#3904=ORIENTED_EDGE('',*,*,#2711,.T.);
#3905=ORIENTED_EDGE('',*,*,#2704,.T.);
#3906=ORIENTED_EDGE('',*,*,#2706,.T.);
#3907=ORIENTED_EDGE('',*,*,#2709,.T.);
#3908=ORIENTED_EDGE('',*,*,#2712,.F.);
#3909=ORIENTED_EDGE('',*,*,#2713,.F.);
#3910=ORIENTED_EDGE('',*,*,#2714,.F.);
#3911=ORIENTED_EDGE('',*,*,#2689,.T.);
#3912=ORIENTED_EDGE('',*,*,#2692,.T.);
#3913=ORIENTED_EDGE('',*,*,#2708,.T.);
#3914=ORIENTED_EDGE('',*,*,#2698,.F.);
#3915=ORIENTED_EDGE('',*,*,#2715,.T.);
#3916=ORIENTED_EDGE('',*,*,#2712,.T.);
#3917=ORIENTED_EDGE('',*,*,#2715,.F.);
#3918=ORIENTED_EDGE('',*,*,#2697,.F.);
#3919=ORIENTED_EDGE('',*,*,#2716,.F.);
#3920=ORIENTED_EDGE('',*,*,#2713,.T.);
#3921=ORIENTED_EDGE('',*,*,#2710,.F.);
#3922=ORIENTED_EDGE('',*,*,#2717,.T.);
#3923=ORIENTED_EDGE('',*,*,#2695,.F.);
#3924=ORIENTED_EDGE('',*,*,#2718,.F.);
#3925=ORIENTED_EDGE('',*,*,#2714,.T.);
#3926=ORIENTED_EDGE('',*,*,#2716,.T.);
#3927=ORIENTED_EDGE('',*,*,#2696,.F.);
#3928=ORIENTED_EDGE('',*,*,#2717,.F.);
#3929=ORIENTED_EDGE('',*,*,#2718,.T.);
#3930=ORIENTED_EDGE('',*,*,#2702,.T.);
#3931=ORIENTED_EDGE('',*,*,#2705,.T.);
#3932=ORIENTED_EDGE('',*,*,#2711,.F.);
#3933=ORIENTED_EDGE('',*,*,#2719,.F.);
#3934=ORIENTED_EDGE('',*,*,#2720,.F.);
#3935=ORIENTED_EDGE('',*,*,#2721,.F.);
#3936=ORIENTED_EDGE('',*,*,#2722,.F.);
#3937=ORIENTED_EDGE('',*,*,#2723,.F.);
#3938=ORIENTED_EDGE('',*,*,#2724,.F.);
#3939=ORIENTED_EDGE('',*,*,#2725,.F.);
#3940=ORIENTED_EDGE('',*,*,#2726,.F.);
#3941=ORIENTED_EDGE('',*,*,#2727,.F.);
#3942=ORIENTED_EDGE('',*,*,#2728,.F.);
#3943=ORIENTED_EDGE('',*,*,#2729,.F.);
#3944=ORIENTED_EDGE('',*,*,#2730,.F.);
#3945=ORIENTED_EDGE('',*,*,#2720,.T.);
#3946=ORIENTED_EDGE('',*,*,#2731,.T.);
#3947=ORIENTED_EDGE('',*,*,#2729,.T.);
#3948=ORIENTED_EDGE('',*,*,#2732,.T.);
#3949=ORIENTED_EDGE('',*,*,#2733,.F.);
#3950=ORIENTED_EDGE('',*,*,#2734,.F.);
#3951=ORIENTED_EDGE('',*,*,#2735,.F.);
#3952=ORIENTED_EDGE('',*,*,#2736,.F.);
#3953=ORIENTED_EDGE('',*,*,#2737,.F.);
#3954=ORIENTED_EDGE('',*,*,#2738,.F.);
#3955=ORIENTED_EDGE('',*,*,#2723,.T.);
#3956=ORIENTED_EDGE('',*,*,#2739,.T.);
#3957=ORIENTED_EDGE('',*,*,#2737,.T.);
#3958=ORIENTED_EDGE('',*,*,#2740,.T.);
#3959=ORIENTED_EDGE('',*,*,#2741,.F.);
#3960=ORIENTED_EDGE('',*,*,#2742,.F.);
#3961=ORIENTED_EDGE('',*,*,#2743,.F.);
#3962=ORIENTED_EDGE('',*,*,#2742,.T.);
#3963=ORIENTED_EDGE('',*,*,#2744,.T.);
#3964=ORIENTED_EDGE('',*,*,#2726,.T.);
#3965=ORIENTED_EDGE('',*,*,#2745,.T.);
#3966=ORIENTED_EDGE('',*,*,#2728,.T.);
#3967=ORIENTED_EDGE('',*,*,#2746,.T.);
#3968=ORIENTED_EDGE('',*,*,#2743,.T.);
#3969=ORIENTED_EDGE('',*,*,#2747,.T.);
#3970=ORIENTED_EDGE('',*,*,#2748,.F.);
#3971=ORIENTED_EDGE('',*,*,#2749,.F.);
#3972=ORIENTED_EDGE('',*,*,#2750,.F.);
#3973=ORIENTED_EDGE('',*,*,#2734,.T.);
#3974=ORIENTED_EDGE('',*,*,#2751,.T.);
#3975=ORIENTED_EDGE('',*,*,#2749,.T.);
#3976=ORIENTED_EDGE('',*,*,#2752,.T.);
#3977=ORIENTED_EDGE('',*,*,#2741,.T.);
#3978=ORIENTED_EDGE('',*,*,#2753,.T.);
#3979=ORIENTED_EDGE('',*,*,#2750,.T.);
#3980=ORIENTED_EDGE('',*,*,#2754,.T.);
#3981=ORIENTED_EDGE('',*,*,#2748,.T.);
#3982=ORIENTED_EDGE('',*,*,#2755,.T.);
#3983=ORIENTED_EDGE('',*,*,#2738,.T.);
#3984=ORIENTED_EDGE('',*,*,#2756,.T.);
#3985=ORIENTED_EDGE('',*,*,#2736,.T.);
#3986=ORIENTED_EDGE('',*,*,#2757,.T.);
#3987=ORIENTED_EDGE('',*,*,#2730,.T.);
#3988=ORIENTED_EDGE('',*,*,#2758,.T.);
#3989=ORIENTED_EDGE('',*,*,#2722,.T.);
#3990=ORIENTED_EDGE('',*,*,#2759,.T.);
#3991=ORIENTED_EDGE('',*,*,#2735,.T.);
#3992=ORIENTED_EDGE('',*,*,#2760,.T.);
#3993=ORIENTED_EDGE('',*,*,#2733,.T.);
#3994=ORIENTED_EDGE('',*,*,#2761,.T.);
#3995=ORIENTED_EDGE('',*,*,#2727,.T.);
#3996=ORIENTED_EDGE('',*,*,#2762,.T.);
#3997=ORIENTED_EDGE('',*,*,#2725,.T.);
#3998=ORIENTED_EDGE('',*,*,#2763,.T.);
#3999=ORIENTED_EDGE('',*,*,#2721,.T.);
#4000=ORIENTED_EDGE('',*,*,#2764,.T.);
#4001=ORIENTED_EDGE('',*,*,#2719,.T.);
#4002=ORIENTED_EDGE('',*,*,#2765,.T.);
#4003=ORIENTED_EDGE('',*,*,#2724,.T.);
#4004=ORIENTED_EDGE('',*,*,#2766,.T.);
#4005=ORIENTED_EDGE('',*,*,#2740,.F.);
#4006=ORIENTED_EDGE('',*,*,#2758,.F.);
#4007=ORIENTED_EDGE('',*,*,#2731,.F.);
#4008=ORIENTED_EDGE('',*,*,#2766,.F.);
#4009=ORIENTED_EDGE('',*,*,#2745,.F.);
#4010=ORIENTED_EDGE('',*,*,#2764,.F.);
#4011=ORIENTED_EDGE('',*,*,#2732,.F.);
#4012=ORIENTED_EDGE('',*,*,#2747,.F.);
#4013=ORIENTED_EDGE('',*,*,#2746,.F.);
#4014=ORIENTED_EDGE('',*,*,#2757,.F.);
#4015=ORIENTED_EDGE('',*,*,#2755,.F.);
#4016=ORIENTED_EDGE('',*,*,#2753,.F.);
#4017=ORIENTED_EDGE('',*,*,#2752,.F.);
#4018=ORIENTED_EDGE('',*,*,#2756,.F.);
#4019=ORIENTED_EDGE('',*,*,#2739,.F.);
#4020=ORIENTED_EDGE('',*,*,#2760,.F.);
#4021=ORIENTED_EDGE('',*,*,#2751,.F.);
#4022=ORIENTED_EDGE('',*,*,#2762,.F.);
#4023=ORIENTED_EDGE('',*,*,#2744,.F.);
#4024=ORIENTED_EDGE('',*,*,#2754,.F.);
#4025=ORIENTED_EDGE('',*,*,#2759,.F.);
#4026=ORIENTED_EDGE('',*,*,#2765,.F.);
#4027=ORIENTED_EDGE('',*,*,#2763,.F.);
#4028=ORIENTED_EDGE('',*,*,#2761,.F.);
#4029=CYLINDRICAL_SURFACE('',#4507,11.05);
#4030=CYLINDRICAL_SURFACE('',#4523,0.5);
#4031=CYLINDRICAL_SURFACE('',#4527,0.5);
#4032=CYLINDRICAL_SURFACE('',#4530,0.5);
#4033=CYLINDRICAL_SURFACE('',#4532,0.5);
#4034=CYLINDRICAL_SURFACE('',#4535,0.5);
#4035=CYLINDRICAL_SURFACE('',#4538,0.5);
#4036=CYLINDRICAL_SURFACE('',#4547,57.5);
#4037=CYLINDRICAL_SURFACE('',#4553,60.5);
#4038=CYLINDRICAL_SURFACE('',#4583,59.5);
#4039=CYLINDRICAL_SURFACE('',#4609,10.5);
#4040=CYLINDRICAL_SURFACE('',#4615,3.4544);
#4041=CYLINDRICAL_SURFACE('',#4617,3.4544);
#4042=CYLINDRICAL_SURFACE('',#4618,3.4544);
#4043=CYLINDRICAL_SURFACE('',#4619,3.4544);
#4044=CYLINDRICAL_SURFACE('',#4620,3.4544);
#4045=CYLINDRICAL_SURFACE('',#4621,3.4544);
#4046=CYLINDRICAL_SURFACE('',#4622,3.4544);
#4047=CYLINDRICAL_SURFACE('',#4623,3.4544);
#4048=CYLINDRICAL_SURFACE('',#4624,3.4544);
#4049=CYLINDRICAL_SURFACE('',#4625,3.4544);
#4050=CYLINDRICAL_SURFACE('',#4626,3.4544);
#4051=CYLINDRICAL_SURFACE('',#4627,3.4544);
#4052=CYLINDRICAL_SURFACE('',#4628,3.4544);
#4053=CYLINDRICAL_SURFACE('',#4629,3.4544);
#4054=CYLINDRICAL_SURFACE('',#4630,3.4544);
#4055=CYLINDRICAL_SURFACE('',#4631,3.4544);
#4056=CYLINDRICAL_SURFACE('',#4632,3.4544);
#4057=CYLINDRICAL_SURFACE('',#4634,3.96875);
#4058=CYLINDRICAL_SURFACE('',#4636,3.96875);
#4059=CYLINDRICAL_SURFACE('',#4637,3.96875);
#4060=CYLINDRICAL_SURFACE('',#4638,3.96875);
#4061=CYLINDRICAL_SURFACE('',#4639,3.96875);
#4062=CYLINDRICAL_SURFACE('',#4640,3.96875);
#4063=CYLINDRICAL_SURFACE('',#4641,3.96875);
#4064=CYLINDRICAL_SURFACE('',#4642,3.96875);
#4065=CYLINDRICAL_SURFACE('',#4643,3.96875);
#4066=CYLINDRICAL_SURFACE('',#4644,3.96875);
#4067=CYLINDRICAL_SURFACE('',#4645,3.96875);
#4068=CYLINDRICAL_SURFACE('',#4646,3.96875);
#4069=CYLINDRICAL_SURFACE('',#4647,3.96875);
#4070=CYLINDRICAL_SURFACE('',#4648,3.96875);
#4071=CYLINDRICAL_SURFACE('',#4649,3.96875);
#4072=CYLINDRICAL_SURFACE('',#4650,3.96875);
#4073=CYLINDRICAL_SURFACE('',#4651,3.96875);
#4074=CYLINDRICAL_SURFACE('',#4652,3.96875);
#4075=CYLINDRICAL_SURFACE('',#4657,3.96875);
#4076=CYLINDRICAL_SURFACE('',#4662,3.4544);
#4077=CYLINDRICAL_SURFACE('',#4682,7.6);
#4078=CYLINDRICAL_SURFACE('',#4686,7.94);
#4079=CYLINDRICAL_SURFACE('',#4690,7.6);
#4080=CYLINDRICAL_SURFACE('',#4694,7.94);
#4081=CYLINDRICAL_SURFACE('',#4699,7.94);
#4082=CYLINDRICAL_SURFACE('',#4715,0.5);
#4083=CYLINDRICAL_SURFACE('',#4736,12.);
#4084=CYLINDRICAL_SURFACE('',#4738,0.5);
#4085=CYLINDRICAL_SURFACE('',#4741,0.5);
#4086=CYLINDRICAL_SURFACE('',#4749,0.5);
#4087=CYLINDRICAL_SURFACE('',#4753,0.5);
#4088=CYLINDRICAL_SURFACE('',#4759,0.5);
#4089=CYLINDRICAL_SURFACE('',#4776,0.5);
#4090=CYLINDRICAL_SURFACE('',#4777,0.5);
#4091=CYLINDRICAL_SURFACE('',#4782,0.5);
#4092=CYLINDRICAL_SURFACE('',#4783,7.95);
#4093=CYLINDRICAL_SURFACE('',#4786,0.5);
#4094=CYLINDRICAL_SURFACE('',#4801,12.6);
#4095=CYLINDRICAL_SURFACE('',#4810,10.5);
#4096=CYLINDRICAL_SURFACE('',#4813,10.5);
#4097=CYLINDRICAL_SURFACE('',#4827,11.);
#4098=CYLINDRICAL_SURFACE('',#4835,11.);
#4099=CYLINDRICAL_SURFACE('',#4853,0.4);
#4100=CYLINDRICAL_SURFACE('',#4857,0.4);
#4101=CYLINDRICAL_SURFACE('',#4868,7.95);
#4102=CYLINDRICAL_SURFACE('',#4880,0.4);
#4103=CYLINDRICAL_SURFACE('',#4883,0.4);
#4104=CYLINDRICAL_SURFACE('',#4900,16.);
#4105=CYLINDRICAL_SURFACE('',#4912,10.5);
#4106=CYLINDRICAL_SURFACE('',#4918,10.5);
#4107=CYLINDRICAL_SURFACE('',#4925,7.965);
#4108=CYLINDRICAL_SURFACE('',#4934,11.);
#4109=CYLINDRICAL_SURFACE('',#4940,8.);
#4110=CYLINDRICAL_SURFACE('',#4944,0.85);
#4111=CYLINDRICAL_SURFACE('',#4947,0.85);
#4112=CYLINDRICAL_SURFACE('',#4959,9.9);
#4113=CYLINDRICAL_SURFACE('',#4963,7.6);
#4114=ADVANCED_FACE('',(#324),#4029,.F.);
#4115=ADVANCED_FACE('',(#325),#298,.F.);
#4116=ADVANCED_FACE('',(#326),#294,.T.);
#4117=ADVANCED_FACE('',(#327),#258,.T.);
#4118=ADVANCED_FACE('',(#328,#141),#169,.T.);
#4119=ADVANCED_FACE('',(#329),#299,.F.);
#4120=ADVANCED_FACE('',(#330),#295,.T.);
#4121=ADVANCED_FACE('',(#331),#300,.T.);
#4122=ADVANCED_FACE('',(#332,#142),#170,.T.);
#4123=ADVANCED_FACE('',(#333),#301,.F.);
#4124=ADVANCED_FACE('',(#334,#143),#171,.T.);
#4125=ADVANCED_FACE('',(#335),#4030,.T.);
#4126=ADVANCED_FACE('',(#336),#302,.F.);
#4127=ADVANCED_FACE('',(#337),#4031,.T.);
#4128=ADVANCED_FACE('',(#338),#303,.F.);
#4129=ADVANCED_FACE('',(#339),#4032,.T.);
#4130=ADVANCED_FACE('',(#340),#172,.F.);
#4131=ADVANCED_FACE('',(#341),#4033,.T.);
#4132=ADVANCED_FACE('',(#342),#304,.F.);
#4133=ADVANCED_FACE('',(#343),#4034,.T.);
#4134=ADVANCED_FACE('',(#344),#305,.F.);
#4135=ADVANCED_FACE('',(#345),#4035,.T.);
#4136=ADVANCED_FACE('',(#346),#173,.F.);
#4137=ADVANCED_FACE('',(#347),#259,.T.);
#4138=ADVANCED_FACE('',(#348),#174,.F.);
#4139=ADVANCED_FACE('',(#349),#260,.T.);
#4140=ADVANCED_FACE('',(#350),#4036,.F.);
#4141=ADVANCED_FACE('',(#351),#261,.T.);
#4142=ADVANCED_FACE('',(#352),#175,.T.);
#4143=ADVANCED_FACE('',(#353),#4037,.T.);
#4144=ADVANCED_FACE('',(#354),#262,.T.);
#4145=ADVANCED_FACE('',(#355),#263,.T.);
#4146=ADVANCED_FACE('',(#356),#264,.T.);
#4147=ADVANCED_FACE('',(#357),#81,.T.);
#4148=ADVANCED_FACE('',(#358,#144),#176,.T.);
#4149=ADVANCED_FACE('',(#359),#265,.T.);
#4150=ADVANCED_FACE('',(#360),#82,.T.);
#4151=ADVANCED_FACE('',(#361),#266,.T.);
#4152=ADVANCED_FACE('',(#362),#4038,.T.);
#4153=ADVANCED_FACE('',(#363),#267,.T.);
#4154=ADVANCED_FACE('',(#364),#83,.T.);
#4155=ADVANCED_FACE('',(#365),#268,.T.);
#4156=ADVANCED_FACE('',(#366),#84,.T.);
#4157=ADVANCED_FACE('',(#367),#269,.T.);
#4158=ADVANCED_FACE('',(#368,#145),#177,.T.);
#4159=ADVANCED_FACE('',(#369),#270,.T.);
#4160=ADVANCED_FACE('',(#370),#4039,.F.);
#4161=ADVANCED_FACE('',(#371),#271,.T.);
#4162=ADVANCED_FACE('',(#372),#4040,.F.);
#4163=ADVANCED_FACE('',(#373),#4041,.F.);
#4164=ADVANCED_FACE('',(#374),#4042,.F.);
#4165=ADVANCED_FACE('',(#375),#4043,.F.);
#4166=ADVANCED_FACE('',(#376),#4044,.F.);
#4167=ADVANCED_FACE('',(#377),#4045,.F.);
#4168=ADVANCED_FACE('',(#378),#4046,.F.);
#4169=ADVANCED_FACE('',(#379),#4047,.F.);
#4170=ADVANCED_FACE('',(#380),#4048,.F.);
#4171=ADVANCED_FACE('',(#381),#4049,.F.);
#4172=ADVANCED_FACE('',(#382),#4050,.F.);
#4173=ADVANCED_FACE('',(#383),#4051,.F.);
#4174=ADVANCED_FACE('',(#384),#4052,.F.);
#4175=ADVANCED_FACE('',(#385),#4053,.F.);
#4176=ADVANCED_FACE('',(#386),#4054,.F.);
#4177=ADVANCED_FACE('',(#387),#4055,.F.);
#4178=ADVANCED_FACE('',(#388),#4056,.F.);
#4179=ADVANCED_FACE('',(#389),#4057,.F.);
#4180=ADVANCED_FACE('',(#390),#4058,.F.);
#4181=ADVANCED_FACE('',(#391),#4059,.F.);
#4182=ADVANCED_FACE('',(#392),#4060,.F.);
#4183=ADVANCED_FACE('',(#393),#4061,.F.);
#4184=ADVANCED_FACE('',(#394),#4062,.F.);
#4185=ADVANCED_FACE('',(#395),#4063,.F.);
#4186=ADVANCED_FACE('',(#396),#4064,.F.);
#4187=ADVANCED_FACE('',(#397),#4065,.F.);
#4188=ADVANCED_FACE('',(#398),#4066,.F.);
#4189=ADVANCED_FACE('',(#399),#4067,.F.);
#4190=ADVANCED_FACE('',(#400),#4068,.F.);
#4191=ADVANCED_FACE('',(#401),#4069,.F.);
#4192=ADVANCED_FACE('',(#402),#4070,.F.);
#4193=ADVANCED_FACE('',(#403),#4071,.F.);
#4194=ADVANCED_FACE('',(#404),#4072,.F.);
#4195=ADVANCED_FACE('',(#405),#4073,.F.);
#4196=ADVANCED_FACE('',(#406),#4074,.F.);
#4197=ADVANCED_FACE('',(#407),#178,.F.);
#4198=ADVANCED_FACE('',(#408),#4075,.F.);
#4199=ADVANCED_FACE('',(#409),#306,.F.);
#4200=ADVANCED_FACE('',(#410),#179,.T.);
#4201=ADVANCED_FACE('',(#411),#307,.F.);
#4202=ADVANCED_FACE('',(#412),#85,.F.);
#4203=ADVANCED_FACE('',(#413),#4076,.F.);
#4204=ADVANCED_FACE('',(#414),#86,.F.);
#4205=ADVANCED_FACE('',(#415),#180,.F.);
#4206=ADVANCED_FACE('',(#416),#181,.F.);
#4207=ADVANCED_FACE('',(#417),#182,.F.);
#4208=ADVANCED_FACE('',(#418),#183,.F.);
#4209=ADVANCED_FACE('',(#419),#184,.F.);
#4210=ADVANCED_FACE('',(#420),#185,.F.);
#4211=ADVANCED_FACE('',(#421),#186,.F.);
#4212=ADVANCED_FACE('',(#422),#187,.F.);
#4213=ADVANCED_FACE('',(#423),#188,.F.);
#4214=ADVANCED_FACE('',(#424),#189,.F.);
#4215=ADVANCED_FACE('',(#425,#146),#190,.F.);
#4216=ADVANCED_FACE('',(#426),#4077,.T.);
#4217=ADVANCED_FACE('',(#427,#147),#191,.F.);
#4218=ADVANCED_FACE('',(#428,#148,#149),#4078,.T.);
#4219=ADVANCED_FACE('',(#429,#150),#192,.F.);
#4220=ADVANCED_FACE('',(#430),#4079,.T.);
#4221=ADVANCED_FACE('',(#431,#151),#193,.F.);
#4222=ADVANCED_FACE('',(#432),#4080,.T.);
#4223=ADVANCED_FACE('',(#433),#194,.T.);
#4224=ADVANCED_FACE('',(#434),#87,.T.);
#4225=ADVANCED_FACE('',(#435),#4081,.T.);
#4226=ADVANCED_FACE('',(#436),#88,.T.);
#4227=ADVANCED_FACE('',(#437,#152),#195,.T.);
#4228=ADVANCED_FACE('',(#438),#272,.T.);
#4229=ADVANCED_FACE('',(#439),#67,.T.);
#4230=ADVANCED_FACE('',(#440),#68,.T.);
#4231=ADVANCED_FACE('',(#441),#308,.F.);
#4232=ADVANCED_FACE('',(#442),#4082,.T.);
#4233=ADVANCED_FACE('',(#443),#196,.T.);
#4234=ADVANCED_FACE('',(#444),#309,.F.);
#4235=ADVANCED_FACE('',(#445),#69,.T.);
#4236=ADVANCED_FACE('',(#446),#70,.T.);
#4237=ADVANCED_FACE('',(#447),#310,.F.);
#4238=ADVANCED_FACE('',(#448),#311,.F.);
#4239=ADVANCED_FACE('',(#449),#296,.T.);
#4240=ADVANCED_FACE('',(#450),#312,.F.);
#4241=ADVANCED_FACE('',(#451),#197,.F.);
#4242=ADVANCED_FACE('',(#452),#313,.F.);
#4243=ADVANCED_FACE('',(#453),#89,.F.);
#4244=ADVANCED_FACE('',(#454),#273,.T.);
#4245=ADVANCED_FACE('',(#455,#153),#198,.T.);
#4246=ADVANCED_FACE('',(#456),#4083,.T.);
#4247=ADVANCED_FACE('',(#457),#4084,.T.);
#4248=ADVANCED_FACE('',(#458),#4085,.T.);
#4249=ADVANCED_FACE('',(#459),#71,.T.);
#4250=ADVANCED_FACE('',(#460),#274,.T.);
#4251=ADVANCED_FACE('',(#461),#4086,.T.);
#4252=ADVANCED_FACE('',(#462),#199,.F.);
#4253=ADVANCED_FACE('',(#463),#200,.F.);
#4254=ADVANCED_FACE('',(#464),#4087,.T.);
#4255=ADVANCED_FACE('',(#465),#72,.T.);
#4256=ADVANCED_FACE('',(#466),#4088,.T.);
#4257=ADVANCED_FACE('',(#467),#275,.T.);
#4258=ADVANCED_FACE('',(#468),#276,.T.);
#4259=ADVANCED_FACE('',(#469,#154),#201,.T.);
#4260=ADVANCED_FACE('',(#470),#90,.T.);
#4261=ADVANCED_FACE('',(#471),#73,.T.);
#4262=ADVANCED_FACE('',(#472),#4089,.T.);
#4263=ADVANCED_FACE('',(#473),#4090,.T.);
#4264=ADVANCED_FACE('',(#474),#74,.T.);
#4265=ADVANCED_FACE('',(#475),#202,.F.);
#4266=ADVANCED_FACE('',(#476),#4091,.T.);
#4267=ADVANCED_FACE('',(#477),#4092,.F.);
#4268=ADVANCED_FACE('',(#478),#314,.F.);
#4269=ADVANCED_FACE('',(#479),#4093,.T.);
#4270=ADVANCED_FACE('',(#480),#75,.T.);
#4271=ADVANCED_FACE('',(#481),#76,.T.);
#4272=ADVANCED_FACE('',(#482),#315,.F.);
#4273=ADVANCED_FACE('',(#483),#297,.T.);
#4274=ADVANCED_FACE('',(#484),#316,.F.);
#4275=ADVANCED_FACE('',(#485),#203,.F.);
#4276=ADVANCED_FACE('',(#486),#317,.F.);
#4277=ADVANCED_FACE('',(#487),#204,.F.);
#4278=ADVANCED_FACE('',(#488),#318,.F.);
#4279=ADVANCED_FACE('',(#489,#155),#205,.T.);
#4280=ADVANCED_FACE('',(#490),#91,.F.);
#4281=ADVANCED_FACE('',(#491),#92,.T.);
#4282=ADVANCED_FACE('',(#492),#4094,.T.);
#4283=ADVANCED_FACE('',(#493,#156),#206,.T.);
#4284=ADVANCED_FACE('',(#494),#93,.T.);
#4285=ADVANCED_FACE('',(#495,#157),#207,.T.);
#4286=ADVANCED_FACE('',(#496),#4095,.F.);
#4287=ADVANCED_FACE('',(#497),#4096,.F.);
#4288=ADVANCED_FACE('',(#498),#208,.T.);
#4289=ADVANCED_FACE('',(#499),#209,.T.);
#4290=ADVANCED_FACE('',(#500),#210,.T.);
#4291=ADVANCED_FACE('',(#501),#211,.T.);
#4292=ADVANCED_FACE('',(#502),#212,.F.);
#4293=ADVANCED_FACE('',(#503),#319,.F.);
#4294=ADVANCED_FACE('',(#504),#277,.T.);
#4295=ADVANCED_FACE('',(#505),#4097,.T.);
#4296=ADVANCED_FACE('',(#506),#94,.T.);
#4297=ADVANCED_FACE('',(#507),#278,.T.);
#4298=ADVANCED_FACE('',(#508),#4098,.T.);
#4299=ADVANCED_FACE('',(#509),#279,.T.);
#4300=ADVANCED_FACE('',(#510),#95,.T.);
#4301=ADVANCED_FACE('',(#511),#320,.F.);
#4302=ADVANCED_FACE('',(#512),#321,.F.);
#4303=ADVANCED_FACE('',(#513),#322,.F.);
#4304=ADVANCED_FACE('',(#514),#323,.F.);
#4305=ADVANCED_FACE('',(#515),#280,.T.);
#4306=ADVANCED_FACE('',(#516),#77,.T.);
#4307=ADVANCED_FACE('',(#517),#78,.T.);
#4308=ADVANCED_FACE('',(#518),#213,.F.);
#4309=ADVANCED_FACE('',(#519),#4099,.T.);
#4310=ADVANCED_FACE('',(#520),#214,.T.);
#4311=ADVANCED_FACE('',(#521),#4100,.T.);
#4312=ADVANCED_FACE('',(#522),#281,.T.);
#4313=ADVANCED_FACE('',(#523,#158),#215,.T.);
#4314=ADVANCED_FACE('',(#524),#282,.T.);
#4315=ADVANCED_FACE('',(#525),#4101,.F.);
#4316=ADVANCED_FACE('',(#526),#216,.F.);
#4317=ADVANCED_FACE('',(#527),#79,.T.);
#4318=ADVANCED_FACE('',(#528),#80,.T.);
#4319=ADVANCED_FACE('',(#529),#283,.T.);
#4320=ADVANCED_FACE('',(#530),#4102,.T.);
#4321=ADVANCED_FACE('',(#531),#284,.T.);
#4322=ADVANCED_FACE('',(#532),#4103,.T.);
#4323=ADVANCED_FACE('',(#533),#217,.F.);
#4324=ADVANCED_FACE('',(#534),#285,.T.);
#4325=ADVANCED_FACE('',(#535),#96,.T.);
#4326=ADVANCED_FACE('',(#536,#159),#218,.T.);
#4327=ADVANCED_FACE('',(#537),#286,.T.);
#4328=ADVANCED_FACE('',(#538),#4104,.T.);
#4329=ADVANCED_FACE('',(#539),#287,.T.);
#4330=ADVANCED_FACE('',(#540,#160),#219,.T.);
#4331=ADVANCED_FACE('',(#541),#288,.T.);
#4332=ADVANCED_FACE('',(#542),#4105,.F.);
#4333=ADVANCED_FACE('',(#543),#289,.T.);
#4334=ADVANCED_FACE('',(#544),#4106,.T.);
#4335=ADVANCED_FACE('',(#545,#161),#220,.T.);
#4336=ADVANCED_FACE('',(#546),#97,.F.);
#4337=ADVANCED_FACE('',(#547),#4107,.F.);
#4338=ADVANCED_FACE('',(#548),#98,.F.);
#4339=ADVANCED_FACE('',(#549,#162),#221,.T.);
#4340=ADVANCED_FACE('',(#550),#99,.T.);
#4341=ADVANCED_FACE('',(#551),#4108,.T.);
#4342=ADVANCED_FACE('',(#552),#100,.T.);
#4343=ADVANCED_FACE('',(#553,#163),#222,.T.);
#4344=ADVANCED_FACE('',(#554),#4109,.F.);
#4345=ADVANCED_FACE('',(#555,#164),#223,.T.);
#4346=ADVANCED_FACE('',(#556),#4110,.F.);
#4347=ADVANCED_FACE('',(#557),#4111,.F.);
#4348=ADVANCED_FACE('',(#558,#165,#166),#224,.T.);
#4349=ADVANCED_FACE('',(#559),#225,.T.);
#4350=ADVANCED_FACE('',(#560),#226,.T.);
#4351=ADVANCED_FACE('',(#561),#227,.T.);
#4352=ADVANCED_FACE('',(#562,#167,#168),#228,.T.);
#4353=ADVANCED_FACE('',(#563),#4112,.T.);
#4354=ADVANCED_FACE('',(#564),#229,.T.);
#4355=ADVANCED_FACE('',(#565),#230,.T.);
#4356=ADVANCED_FACE('',(#566),#231,.T.);
#4357=ADVANCED_FACE('',(#567),#4113,.F.);
#4358=ADVANCED_FACE('',(#568),#232,.T.);
#4359=ADVANCED_FACE('',(#569),#233,.T.);
#4360=ADVANCED_FACE('',(#570),#234,.T.);
#4361=ADVANCED_FACE('',(#571),#235,.T.);
#4362=ADVANCED_FACE('',(#572),#236,.T.);
#4363=ADVANCED_FACE('',(#573),#237,.T.);
#4364=ADVANCED_FACE('',(#574),#238,.T.);
#4365=ADVANCED_FACE('',(#575),#239,.T.);
#4366=ADVANCED_FACE('',(#576),#240,.T.);
#4367=ADVANCED_FACE('',(#577),#241,.T.);
#4368=ADVANCED_FACE('',(#578),#242,.T.);
#4369=ADVANCED_FACE('',(#579),#243,.T.);
#4370=ADVANCED_FACE('',(#580),#244,.T.);
#4371=ADVANCED_FACE('',(#581),#245,.T.);
#4372=ADVANCED_FACE('',(#582),#246,.T.);
#4373=ADVANCED_FACE('',(#583),#247,.T.);
#4374=ADVANCED_FACE('',(#584),#248,.T.);
#4375=ADVANCED_FACE('',(#585),#249,.T.);
#4376=ADVANCED_FACE('',(#586),#250,.T.);
#4377=ADVANCED_FACE('',(#587),#251,.T.);
#4378=ADVANCED_FACE('',(#588),#252,.T.);
#4379=ADVANCED_FACE('',(#589),#253,.T.);
#4380=ADVANCED_FACE('',(#590),#254,.T.);
#4381=ADVANCED_FACE('',(#591),#255,.T.);
#4382=ADVANCED_FACE('',(#592),#256,.T.);
#4383=ADVANCED_FACE('',(#593),#257,.T.);
#4384=CLOSED_SHELL('',(#4114,#4115,#4116,#4117,#4118,#4119,#4120,#4121,
#4122,#4123,#4124,#4125,#4126,#4127,#4128,#4129,#4130,#4131,#4132,#4133,
#4134,#4135,#4136,#4137,#4138,#4139,#4140,#4141,#4142,#4143,#4144,#4145));
#4385=CLOSED_SHELL('',(#4146,#4147,#4148,#4149,#4150,#4151,#4152,#4153,
#4154,#4155,#4156,#4157,#4158,#4159,#4160,#4161));
#4386=CLOSED_SHELL('',(#4162,#4163,#4164,#4165,#4166,#4167,#4168,#4169,
#4170,#4171,#4172,#4173,#4174,#4175,#4176,#4177,#4178,#4179,#4180,#4181,
#4182,#4183,#4184,#4185,#4186,#4187,#4188,#4189,#4190,#4191,#4192,#4193,
#4194,#4195,#4196,#4197,#4198,#4199,#4200,#4201,#4202,#4203,#4204,#4205,
#4206,#4207,#4208,#4209,#4210,#4211,#4212,#4213,#4214,#4215,#4216,#4217,
#4218,#4219,#4220,#4221,#4222,#4223,#4224,#4225,#4226,#4227));
#4387=CLOSED_SHELL('',(#4228,#4229,#4230,#4231,#4232,#4233,#4234,#4235,
#4236,#4237,#4238,#4239,#4240,#4241,#4242,#4243,#4244,#4245,#4246,#4247,
#4248,#4249,#4250,#4251,#4252,#4253,#4254,#4255,#4256,#4257,#4258,#4259,
#4260,#4261,#4262,#4263,#4264,#4265,#4266,#4267,#4268,#4269,#4270,#4271,
#4272,#4273,#4274,#4275,#4276,#4277,#4278,#4279,#4280));
#4388=CLOSED_SHELL('',(#4281,#4282,#4283,#4284,#4285,#4286,#4287,#4288,
#4289,#4290,#4291,#4292,#4293,#4294,#4295,#4296,#4297,#4298,#4299,#4300,
#4301,#4302,#4303,#4304,#4305,#4306,#4307,#4308,#4309,#4310,#4311,#4312,
#4313,#4314,#4315,#4316,#4317,#4318,#4319,#4320,#4321,#4322,#4323));
#4389=CLOSED_SHELL('',(#4324,#4325,#4326,#4327,#4328,#4329,#4330,#4331,
#4332,#4333));
#4390=CLOSED_SHELL('',(#4334,#4335,#4336,#4337,#4338,#4339));
#4391=CLOSED_SHELL('',(#4340,#4341,#4342,#4343,#4344,#4345));
#4392=CLOSED_SHELL('',(#4346,#4347,#4348,#4349,#4350,#4351,#4352,#4353,
#4354,#4355,#4356,#4357));
#4393=CLOSED_SHELL('',(#4358,#4359,#4360,#4361,#4362,#4363,#4364,#4365,
#4366,#4367,#4368,#4369,#4370,#4371,#4372,#4373,#4374,#4375,#4376,#4377,
#4378,#4379,#4380,#4381,#4382,#4383));
#4394=DERIVED_UNIT_ELEMENT(#4414,1.);
#4395=DERIVED_UNIT_ELEMENT(#12815,-3.);
#4396=DERIVED_UNIT_ELEMENT(#4414,1.);
#4397=DERIVED_UNIT_ELEMENT(#12815,-3.);
#4398=DERIVED_UNIT_ELEMENT(#4414,1.);
#4399=DERIVED_UNIT_ELEMENT(#12815,-3.);
#4400=DERIVED_UNIT_ELEMENT(#4414,1.);
#4401=DERIVED_UNIT_ELEMENT(#12815,-3.);
#4402=DERIVED_UNIT_ELEMENT(#4414,1.);
#4403=DERIVED_UNIT_ELEMENT(#12815,-3.);
#4404=DERIVED_UNIT_ELEMENT(#4414,1.);
#4405=DERIVED_UNIT_ELEMENT(#12815,-3.);
#4406=DERIVED_UNIT_ELEMENT(#4414,1.);
#4407=DERIVED_UNIT_ELEMENT(#12815,-3.);
#4408=DERIVED_UNIT_ELEMENT(#4414,1.);
#4409=DERIVED_UNIT_ELEMENT(#12815,-3.);
#4410=DERIVED_UNIT_ELEMENT(#4414,1.);
#4411=DERIVED_UNIT_ELEMENT(#12815,-3.);
#4412=DERIVED_UNIT_ELEMENT(#4414,1.);
#4413=DERIVED_UNIT_ELEMENT(#12815,-3.);
#4414=(
MASS_UNIT()
NAMED_UNIT(*)
SI_UNIT(.KILO.,.GRAM.)
);
#4415=DERIVED_UNIT((#4394,#4395));
#4416=DERIVED_UNIT((#4396,#4397));
#4417=DERIVED_UNIT((#4398,#4399));
#4418=DERIVED_UNIT((#4400,#4401));
#4419=DERIVED_UNIT((#4402,#4403));
#4420=DERIVED_UNIT((#4404,#4405));
#4421=DERIVED_UNIT((#4406,#4407));
#4422=DERIVED_UNIT((#4408,#4409));
#4423=DERIVED_UNIT((#4410,#4411));
#4424=DERIVED_UNIT((#4412,#4413));
#4425=MEASURE_REPRESENTATION_ITEM('density measure',
POSITIVE_RATIO_MEASURE(7850.),#4415);
#4426=MEASURE_REPRESENTATION_ITEM('density measure',
POSITIVE_RATIO_MEASURE(7850.),#4416);
#4427=MEASURE_REPRESENTATION_ITEM('density measure',
POSITIVE_RATIO_MEASURE(7850.),#4417);
#4428=MEASURE_REPRESENTATION_ITEM('density measure',
POSITIVE_RATIO_MEASURE(7850.),#4418);
#4429=MEASURE_REPRESENTATION_ITEM('density measure',
POSITIVE_RATIO_MEASURE(7850.),#4419);
#4430=MEASURE_REPRESENTATION_ITEM('density measure',
POSITIVE_RATIO_MEASURE(7850.),#4420);
#4431=MEASURE_REPRESENTATION_ITEM('density measure',
POSITIVE_RATIO_MEASURE(7850.),#4421);
#4432=MEASURE_REPRESENTATION_ITEM('density measure',
POSITIVE_RATIO_MEASURE(7850.),#4422);
#4433=MEASURE_REPRESENTATION_ITEM('density measure',
POSITIVE_RATIO_MEASURE(7850.),#4423);
#4434=MEASURE_REPRESENTATION_ITEM('density measure',
POSITIVE_RATIO_MEASURE(7850.),#4424);
#4435=PROPERTY_DEFINITION_REPRESENTATION(#4485,#4455);
#4436=PROPERTY_DEFINITION_REPRESENTATION(#4486,#4456);
#4437=PROPERTY_DEFINITION_REPRESENTATION(#4487,#4457);
#4438=PROPERTY_DEFINITION_REPRESENTATION(#4488,#4458);
#4439=PROPERTY_DEFINITION_REPRESENTATION(#4489,#4459);
#4440=PROPERTY_DEFINITION_REPRESENTATION(#4490,#4460);
#4441=PROPERTY_DEFINITION_REPRESENTATION(#4491,#4461);
#4442=PROPERTY_DEFINITION_REPRESENTATION(#4492,#4462);
#4443=PROPERTY_DEFINITION_REPRESENTATION(#4493,#4463);
#4444=PROPERTY_DEFINITION_REPRESENTATION(#4494,#4464);
#4445=PROPERTY_DEFINITION_REPRESENTATION(#4495,#4465);
#4446=PROPERTY_DEFINITION_REPRESENTATION(#4496,#4466);
#4447=PROPERTY_DEFINITION_REPRESENTATION(#4497,#4467);
#4448=PROPERTY_DEFINITION_REPRESENTATION(#4498,#4468);
#4449=PROPERTY_DEFINITION_REPRESENTATION(#4499,#4469);
#4450=PROPERTY_DEFINITION_REPRESENTATION(#4500,#4470);
#4451=PROPERTY_DEFINITION_REPRESENTATION(#4501,#4471);
#4452=PROPERTY_DEFINITION_REPRESENTATION(#4502,#4472);
#4453=PROPERTY_DEFINITION_REPRESENTATION(#4503,#4473);
#4454=PROPERTY_DEFINITION_REPRESENTATION(#4504,#4474);
#4455=REPRESENTATION('material name',(#4475),#12803);
#4456=REPRESENTATION('density',(#4425),#12803);
#4457=REPRESENTATION('material name',(#4476),#12804);
#4458=REPRESENTATION('density',(#4426),#12804);
#4459=REPRESENTATION('material name',(#4477),#12805);
#4460=REPRESENTATION('density',(#4427),#12805);
#4461=REPRESENTATION('material name',(#4478),#12806);
#4462=REPRESENTATION('density',(#4428),#12806);
#4463=REPRESENTATION('material name',(#4479),#12807);
#4464=REPRESENTATION('density',(#4429),#12807);
#4465=REPRESENTATION('material name',(#4480),#12808);
#4466=REPRESENTATION('density',(#4430),#12808);
#4467=REPRESENTATION('material name',(#4481),#12809);
#4468=REPRESENTATION('density',(#4431),#12809);
#4469=REPRESENTATION('material name',(#4482),#12810);
#4470=REPRESENTATION('density',(#4432),#12810);
#4471=REPRESENTATION('material name',(#4483),#12811);
#4472=REPRESENTATION('density',(#4433),#12811);
#4473=REPRESENTATION('material name',(#4484),#12812);
#4474=REPRESENTATION('density',(#4434),#12812);
#4475=DESCRIPTIVE_REPRESENTATION_ITEM('Steel','Steel');
#4476=DESCRIPTIVE_REPRESENTATION_ITEM('Steel','Steel');
#4477=DESCRIPTIVE_REPRESENTATION_ITEM('Steel','Steel');
#4478=DESCRIPTIVE_REPRESENTATION_ITEM('Steel','Steel');
#4479=DESCRIPTIVE_REPRESENTATION_ITEM('Steel','Steel');
#4480=DESCRIPTIVE_REPRESENTATION_ITEM('Steel','Steel');
#4481=DESCRIPTIVE_REPRESENTATION_ITEM('Steel','Steel');
#4482=DESCRIPTIVE_REPRESENTATION_ITEM('Steel','Steel');
#4483=DESCRIPTIVE_REPRESENTATION_ITEM('Steel','Steel');
#4484=DESCRIPTIVE_REPRESENTATION_ITEM('Steel','Steel');
#4485=PROPERTY_DEFINITION('material property','material name',#12866);
#4486=PROPERTY_DEFINITION('material property','density of part',#12866);
#4487=PROPERTY_DEFINITION('material property','material name',#12867);
#4488=PROPERTY_DEFINITION('material property','density of part',#12867);
#4489=PROPERTY_DEFINITION('material property','material name',#12868);
#4490=PROPERTY_DEFINITION('material property','density of part',#12868);
#4491=PROPERTY_DEFINITION('material property','material name',#12869);
#4492=PROPERTY_DEFINITION('material property','density of part',#12869);
#4493=PROPERTY_DEFINITION('material property','material name',#12870);
#4494=PROPERTY_DEFINITION('material property','density of part',#12870);
#4495=PROPERTY_DEFINITION('material property','material name',#12871);
#4496=PROPERTY_DEFINITION('material property','density of part',#12871);
#4497=PROPERTY_DEFINITION('material property','material name',#12872);
#4498=PROPERTY_DEFINITION('material property','density of part',#12872);
#4499=PROPERTY_DEFINITION('material property','material name',#12873);
#4500=PROPERTY_DEFINITION('material property','density of part',#12873);
#4501=PROPERTY_DEFINITION('material property','material name',#12874);
#4502=PROPERTY_DEFINITION('material property','density of part',#12874);
#4503=PROPERTY_DEFINITION('material property','material name',#12875);
#4504=PROPERTY_DEFINITION('material property','density of part',#12875);
#4505=AXIS2_PLACEMENT_3D('',#6232,#5004,#5005);
#4506=AXIS2_PLACEMENT_3D('',#6233,#5006,#5007);
#4507=AXIS2_PLACEMENT_3D('',#6234,#5008,#5009);
#4508=AXIS2_PLACEMENT_3D('',#6287,#5011,#5012);
#4509=AXIS2_PLACEMENT_3D('',#6288,#5013,#5014);
#4510=AXIS2_PLACEMENT_3D('',#6358,#5015,#5016);
#4511=AXIS2_PLACEMENT_3D('',#6696,#5017,#5018);
#4512=AXIS2_PLACEMENT_3D('',#6698,#5019,#5020);
#4513=AXIS2_PLACEMENT_3D('',#6699,#5021,#5022);
#4514=AXIS2_PLACEMENT_3D('',#6700,#5023,#5024);
#4515=AXIS2_PLACEMENT_3D('',#6788,#5025,#5026);
#4516=AXIS2_PLACEMENT_3D('',#7203,#5027,#5028);
#4517=AXIS2_PLACEMENT_3D('',#7223,#5029,#5030);
#4518=AXIS2_PLACEMENT_3D('',#7226,#5031,#5032);
#4519=AXIS2_PLACEMENT_3D('',#7227,#5033,#5034);
#4520=AXIS2_PLACEMENT_3D('',#7305,#5035,#5036);
#4521=AXIS2_PLACEMENT_3D('',#7355,#5037,#5038);
#4522=AXIS2_PLACEMENT_3D('',#7357,#5039,#5040);
#4523=AXIS2_PLACEMENT_3D('',#7358,#5041,#5042);
#4524=AXIS2_PLACEMENT_3D('',#7361,#5043,#5044);
#4525=AXIS2_PLACEMENT_3D('',#7365,#5046,#5047);
#4526=AXIS2_PLACEMENT_3D('',#7409,#5049,#5050);
#4527=AXIS2_PLACEMENT_3D('',#7420,#5051,#5052);
#4528=AXIS2_PLACEMENT_3D('',#7423,#5053,#5054);
#4529=AXIS2_PLACEMENT_3D('',#7453,#5057,#5058);
#4530=AXIS2_PLACEMENT_3D('',#7464,#5059,#5060);
#4531=AXIS2_PLACEMENT_3D('',#7482,#5063,#5064);
#4532=AXIS2_PLACEMENT_3D('',#7489,#5066,#5067);
#4533=AXIS2_PLACEMENT_3D('',#7508,#5069,#5070);
#4534=AXIS2_PLACEMENT_3D('',#7537,#5072,#5073);
#4535=AXIS2_PLACEMENT_3D('',#7548,#5074,#5075);
#4536=AXIS2_PLACEMENT_3D('',#7551,#5076,#5077);
#4537=AXIS2_PLACEMENT_3D('',#7581,#5080,#5081);
#4538=AXIS2_PLACEMENT_3D('',#7592,#5082,#5083);
#4539=AXIS2_PLACEMENT_3D('',#7612,#5086,#5087);
#4540=AXIS2_PLACEMENT_3D('',#7613,#5088,#5089);
#4541=AXIS2_PLACEMENT_3D('',#7620,#5091,#5092);
#4542=AXIS2_PLACEMENT_3D('',#7621,#5093,#5094);
#4543=AXIS2_PLACEMENT_3D('',#7622,#5095,#5096);
#4544=AXIS2_PLACEMENT_3D('',#7623,#5097,#5098);
#4545=AXIS2_PLACEMENT_3D('',#7624,#5099,#5100);
#4546=AXIS2_PLACEMENT_3D('',#7625,#5101,#5102);
#4547=AXIS2_PLACEMENT_3D('',#7626,#5103,#5104);
#4548=AXIS2_PLACEMENT_3D('',#7627,#5105,#5106);
#4549=AXIS2_PLACEMENT_3D('',#7628,#5107,#5108);
#4550=AXIS2_PLACEMENT_3D('',#7629,#5109,#5110);
#4551=AXIS2_PLACEMENT_3D('',#7630,#5111,#5112);
#4552=AXIS2_PLACEMENT_3D('',#7631,#5113,#5114);
#4553=AXIS2_PLACEMENT_3D('',#7632,#5115,#5116);
#4554=AXIS2_PLACEMENT_3D('',#7634,#5117,#5118);
#4555=AXIS2_PLACEMENT_3D('',#7638,#5120,#5121);
#4556=AXIS2_PLACEMENT_3D('',#7639,#5122,#5123);
#4557=AXIS2_PLACEMENT_3D('',#7640,#5124,#5125);
#4558=AXIS2_PLACEMENT_3D('',#7641,#5126,#5127);
#4559=AXIS2_PLACEMENT_3D('',#7642,#5128,#5129);
#4560=AXIS2_PLACEMENT_3D('',#7643,#5130,#5131);
#4561=AXIS2_PLACEMENT_3D('',#7644,#5132,#5133);
#4562=AXIS2_PLACEMENT_3D('',#7645,#5134,#5135);
#4563=AXIS2_PLACEMENT_3D('',#7647,#5136,#5137);
#4564=AXIS2_PLACEMENT_3D('',#7649,#5138,#5139);
#4565=AXIS2_PLACEMENT_3D('',#7651,#5140,#5141);
#4566=AXIS2_PLACEMENT_3D('',#7652,#5142,#5143);
#4567=AXIS2_PLACEMENT_3D('',#7653,#5144,#5145);
#4568=AXIS2_PLACEMENT_3D('',#7657,#5147,#5148);
#4569=AXIS2_PLACEMENT_3D('',#7658,#5149,#5150);
#4570=AXIS2_PLACEMENT_3D('',#7659,#5151,#5152);
#4571=AXIS2_PLACEMENT_3D('',#7661,#5153,#5154);
#4572=AXIS2_PLACEMENT_3D('',#7662,#5155,#5156);
#4573=AXIS2_PLACEMENT_3D('',#7664,#5157,#5158);
#4574=AXIS2_PLACEMENT_3D('',#7666,#5159,#5160);
#4575=AXIS2_PLACEMENT_3D('',#7667,#5161,#5162);
#4576=AXIS2_PLACEMENT_3D('',#7668,#5163,#5164);
#4577=AXIS2_PLACEMENT_3D('',#7672,#5166,#5167);
#4578=AXIS2_PLACEMENT_3D('',#7673,#5168,#5169);
#4579=AXIS2_PLACEMENT_3D('',#7674,#5170,#5171);
#4580=AXIS2_PLACEMENT_3D('',#7676,#5172,#5173);
#4581=AXIS2_PLACEMENT_3D('',#7678,#5174,#5175);
#4582=AXIS2_PLACEMENT_3D('',#7679,#5176,#5177);
#4583=AXIS2_PLACEMENT_3D('',#7680,#5178,#5179);
#4584=AXIS2_PLACEMENT_3D('',#7684,#5181,#5182);
#4585=AXIS2_PLACEMENT_3D('',#7685,#5183,#5184);
#4586=AXIS2_PLACEMENT_3D('',#7686,#5185,#5186);
#4587=AXIS2_PLACEMENT_3D('',#7688,#5187,#5188);
#4588=AXIS2_PLACEMENT_3D('',#7690,#5189,#5190);
#4589=AXIS2_PLACEMENT_3D('',#7691,#5191,#5192);
#4590=AXIS2_PLACEMENT_3D('',#7692,#5193,#5194);
#4591=AXIS2_PLACEMENT_3D('',#7696,#5196,#5197);
#4592=AXIS2_PLACEMENT_3D('',#7697,#5198,#5199);
#4593=AXIS2_PLACEMENT_3D('',#7698,#5200,#5201);
#4594=AXIS2_PLACEMENT_3D('',#7700,#5202,#5203);
#4595=AXIS2_PLACEMENT_3D('',#7702,#5204,#5205);
#4596=AXIS2_PLACEMENT_3D('',#7703,#5206,#5207);
#4597=AXIS2_PLACEMENT_3D('',#7704,#5208,#5209);
#4598=AXIS2_PLACEMENT_3D('',#7708,#5211,#5212);
#4599=AXIS2_PLACEMENT_3D('',#7709,#5213,#5214);
#4600=AXIS2_PLACEMENT_3D('',#7710,#5215,#5216);
#4601=AXIS2_PLACEMENT_3D('',#7712,#5217,#5218);
#4602=AXIS2_PLACEMENT_3D('',#7713,#5219,#5220);
#4603=AXIS2_PLACEMENT_3D('',#7714,#5221,#5222);
#4604=AXIS2_PLACEMENT_3D('',#7716,#5223,#5224);
#4605=AXIS2_PLACEMENT_3D('',#7717,#5225,#5226);
#4606=AXIS2_PLACEMENT_3D('',#7719,#5227,#5228);
#4607=AXIS2_PLACEMENT_3D('',#7721,#5229,#5230);
#4608=AXIS2_PLACEMENT_3D('',#7722,#5231,#5232);
#4609=AXIS2_PLACEMENT_3D('',#7723,#5233,#5234);
#4610=AXIS2_PLACEMENT_3D('',#7726,#5235,#5236);
#4611=AXIS2_PLACEMENT_3D('',#7727,#5237,#5238);
#4612=AXIS2_PLACEMENT_3D('',#7729,#5240,#5241);
#4613=AXIS2_PLACEMENT_3D('',#7730,#5242,#5243);
#4614=AXIS2_PLACEMENT_3D('',#7731,#5244,#5245);
#4615=AXIS2_PLACEMENT_3D('',#7732,#5246,#5247);
#4616=AXIS2_PLACEMENT_3D('',#7751,#5249,#5250);
#4617=AXIS2_PLACEMENT_3D('',#7774,#5251,#5252);
#4618=AXIS2_PLACEMENT_3D('',#7822,#5254,#5255);
#4619=AXIS2_PLACEMENT_3D('',#7873,#5257,#5258);
#4620=AXIS2_PLACEMENT_3D('',#7924,#5260,#5261);
#4621=AXIS2_PLACEMENT_3D('',#7972,#5263,#5264);
#4622=AXIS2_PLACEMENT_3D('',#8023,#5266,#5267);
#4623=AXIS2_PLACEMENT_3D('',#8071,#5269,#5270);
#4624=AXIS2_PLACEMENT_3D('',#8122,#5272,#5273);
#4625=AXIS2_PLACEMENT_3D('',#8173,#5275,#5276);
#4626=AXIS2_PLACEMENT_3D('',#8221,#5278,#5279);
#4627=AXIS2_PLACEMENT_3D('',#8272,#5281,#5282);
#4628=AXIS2_PLACEMENT_3D('',#8323,#5284,#5285);
#4629=AXIS2_PLACEMENT_3D('',#8371,#5287,#5288);
#4630=AXIS2_PLACEMENT_3D('',#8422,#5290,#5291);
#4631=AXIS2_PLACEMENT_3D('',#8470,#5293,#5294);
#4632=AXIS2_PLACEMENT_3D('',#8521,#5296,#5297);
#4633=AXIS2_PLACEMENT_3D('',#8540,#5299,#5300);
#4634=AXIS2_PLACEMENT_3D('',#8563,#5301,#5302);
#4635=AXIS2_PLACEMENT_3D('',#8573,#5304,#5305);
#4636=AXIS2_PLACEMENT_3D('',#8580,#5306,#5307);
#4637=AXIS2_PLACEMENT_3D('',#8605,#5309,#5310);
#4638=AXIS2_PLACEMENT_3D('',#8630,#5312,#5313);
#4639=AXIS2_PLACEMENT_3D('',#8654,#5315,#5316);
#4640=AXIS2_PLACEMENT_3D('',#8679,#5318,#5319);
#4641=AXIS2_PLACEMENT_3D('',#8704,#5321,#5322);
#4642=AXIS2_PLACEMENT_3D('',#8728,#5324,#5325);
#4643=AXIS2_PLACEMENT_3D('',#8752,#5327,#5328);
#4644=AXIS2_PLACEMENT_3D('',#8778,#5330,#5331);
#4645=AXIS2_PLACEMENT_3D('',#8802,#5333,#5334);
#4646=AXIS2_PLACEMENT_3D('',#8826,#5336,#5337);
#4647=AXIS2_PLACEMENT_3D('',#8852,#5339,#5340);
#4648=AXIS2_PLACEMENT_3D('',#8876,#5342,#5343);
#4649=AXIS2_PLACEMENT_3D('',#8900,#5345,#5346);
#4650=AXIS2_PLACEMENT_3D('',#8925,#5348,#5349);
#4651=AXIS2_PLACEMENT_3D('',#8950,#5351,#5352);
#4652=AXIS2_PLACEMENT_3D('',#8974,#5354,#5355);
#4653=AXIS2_PLACEMENT_3D('',#8985,#5357,#5358);
#4654=AXIS2_PLACEMENT_3D('',#8992,#5359,#5360);
#4655=AXIS2_PLACEMENT_3D('',#8994,#5361,#5362);
#4656=AXIS2_PLACEMENT_3D('',#8995,#5363,#5364);
#4657=AXIS2_PLACEMENT_3D('',#9160,#5365,#5366);
#4658=AXIS2_PLACEMENT_3D('',#9749,#5367,#5368);
#4659=AXIS2_PLACEMENT_3D('',#9833,#5369,#5370);
#4660=AXIS2_PLACEMENT_3D('',#9834,#5371,#5372);
#4661=AXIS2_PLACEMENT_3D('',#10317,#5373,#5374);
#4662=AXIS2_PLACEMENT_3D('',#10320,#5376,#5377);
#4663=AXIS2_PLACEMENT_3D('',#10321,#5378,#5379);
#4664=AXIS2_PLACEMENT_3D('',#10324,#5381,#5382);
#4665=AXIS2_PLACEMENT_3D('',#10325,#5383,#5384);
#4666=AXIS2_PLACEMENT_3D('',#10334,#5389,#5390);
#4667=AXIS2_PLACEMENT_3D('',#10336,#5391,#5392);
#4668=AXIS2_PLACEMENT_3D('',#10340,#5395,#5396);
#4669=AXIS2_PLACEMENT_3D('',#10346,#5400,#5401);
#4670=AXIS2_PLACEMENT_3D('',#10347,#5402,#5403);
#4671=AXIS2_PLACEMENT_3D('',#10349,#5405,#5406);
#4672=AXIS2_PLACEMENT_3D('',#10350,#5407,#5408);
#4673=AXIS2_PLACEMENT_3D('',#10359,#5413,#5414);
#4674=AXIS2_PLACEMENT_3D('',#10361,#5415,#5416);
#4675=AXIS2_PLACEMENT_3D('',#10365,#5419,#5420);
#4676=AXIS2_PLACEMENT_3D('',#10371,#5424,#5425);
#4677=AXIS2_PLACEMENT_3D('',#10372,#5426,#5427);
#4678=AXIS2_PLACEMENT_3D('',#10374,#5429,#5430);
#4679=AXIS2_PLACEMENT_3D('',#10375,#5431,#5432);
#4680=AXIS2_PLACEMENT_3D('',#10377,#5433,#5434);
#4681=AXIS2_PLACEMENT_3D('',#10379,#5435,#5436);
#4682=AXIS2_PLACEMENT_3D('',#10380,#5437,#5438);
#4683=AXIS2_PLACEMENT_3D('',#10382,#5439,#5440);
#4684=AXIS2_PLACEMENT_3D('',#10384,#5442,#5443);
#4685=AXIS2_PLACEMENT_3D('',#10386,#5444,#5445);
#4686=AXIS2_PLACEMENT_3D('',#10387,#5446,#5447);
#4687=AXIS2_PLACEMENT_3D('',#10390,#5449,#5450);
#4688=AXIS2_PLACEMENT_3D('',#10391,#5451,#5452);
#4689=AXIS2_PLACEMENT_3D('',#10393,#5453,#5454);
#4690=AXIS2_PLACEMENT_3D('',#10394,#5455,#5456);
#4691=AXIS2_PLACEMENT_3D('',#10396,#5457,#5458);
#4692=AXIS2_PLACEMENT_3D('',#10398,#5460,#5461);
#4693=AXIS2_PLACEMENT_3D('',#10400,#5462,#5463);
#4694=AXIS2_PLACEMENT_3D('',#10401,#5464,#5465);
#4695=AXIS2_PLACEMENT_3D('',#10404,#5467,#5468);
#4696=AXIS2_PLACEMENT_3D('',#10405,#5469,#5470);
#4697=AXIS2_PLACEMENT_3D('',#10407,#5471,#5472);
#4698=AXIS2_PLACEMENT_3D('',#10408,#5473,#5474);
#4699=AXIS2_PLACEMENT_3D('',#10410,#5476,#5477);
#4700=AXIS2_PLACEMENT_3D('',#10412,#5478,#5479);
#4701=AXIS2_PLACEMENT_3D('',#10414,#5481,#5482);
#4702=AXIS2_PLACEMENT_3D('',#10416,#5483,#5484);
#4703=AXIS2_PLACEMENT_3D('',#10418,#5486,#5487);
#4704=AXIS2_PLACEMENT_3D('',#10419,#5488,#5489);
#4705=AXIS2_PLACEMENT_3D('',#10420,#5490,#5491);
#4706=AXIS2_PLACEMENT_3D('',#10423,#5492,#5493);
#4707=AXIS2_PLACEMENT_3D('',#10425,#5494,#5495);
#4708=AXIS2_PLACEMENT_3D('',#10427,#5496,#5497);
#4709=AXIS2_PLACEMENT_3D('',#10428,#5498,#5499);
#4710=AXIS2_PLACEMENT_3D('',#10429,#5500,#5501);
#4711=AXIS2_PLACEMENT_3D('',#10436,#5502,#5503);
#4712=AXIS2_PLACEMENT_3D('',#10437,#5504,#5505);
#4713=AXIS2_PLACEMENT_3D('',#10444,#5506,#5507);
#4714=AXIS2_PLACEMENT_3D('',#10471,#5508,#5509);
#4715=AXIS2_PLACEMENT_3D('',#10476,#5510,#5511);
#4716=AXIS2_PLACEMENT_3D('',#10480,#5513,#5514);
#4717=AXIS2_PLACEMENT_3D('',#10482,#5516,#5517);
#4718=AXIS2_PLACEMENT_3D('',#10596,#5519,#5520);
#4719=AXIS2_PLACEMENT_3D('',#10620,#5521,#5522);
#4720=AXIS2_PLACEMENT_3D('',#10643,#5523,#5524);
#4721=AXIS2_PLACEMENT_3D('',#10645,#5525,#5526);
#4722=AXIS2_PLACEMENT_3D('',#10646,#5527,#5528);
#4723=AXIS2_PLACEMENT_3D('',#10647,#5529,#5530);
#4724=AXIS2_PLACEMENT_3D('',#10648,#5531,#5532);
#4725=AXIS2_PLACEMENT_3D('',#11006,#5533,#5534);
#4726=AXIS2_PLACEMENT_3D('',#11106,#5536,#5537);
#4727=AXIS2_PLACEMENT_3D('',#11135,#5538,#5539);
#4728=AXIS2_PLACEMENT_3D('',#11137,#5540,#5541);
#4729=AXIS2_PLACEMENT_3D('',#11139,#5543,#5544);
#4730=AXIS2_PLACEMENT_3D('',#11142,#5545,#5546);
#4731=AXIS2_PLACEMENT_3D('',#11143,#5547,#5548);
#4732=AXIS2_PLACEMENT_3D('',#11145,#5549,#5550);
#4733=AXIS2_PLACEMENT_3D('',#11146,#5551,#5552);
#4734=AXIS2_PLACEMENT_3D('',#11147,#5553,#5554);
#4735=AXIS2_PLACEMENT_3D('',#11152,#5556,#5557);
#4736=AXIS2_PLACEMENT_3D('',#11156,#5560,#5561);
#4737=AXIS2_PLACEMENT_3D('',#11158,#5562,#5563);
#4738=AXIS2_PLACEMENT_3D('',#11160,#5565,#5566);
#4739=AXIS2_PLACEMENT_3D('',#11162,#5567,#5568);
#4740=AXIS2_PLACEMENT_3D('',#11165,#5570,#5571);
#4741=AXIS2_PLACEMENT_3D('',#11166,#5572,#5573);
#4742=AXIS2_PLACEMENT_3D('',#11169,#5575,#5576);
#4743=AXIS2_PLACEMENT_3D('',#11170,#5577,#5578);
#4744=AXIS2_PLACEMENT_3D('',#11172,#5579,#5580);
#4745=AXIS2_PLACEMENT_3D('',#11173,#5581,#5582);
#4746=AXIS2_PLACEMENT_3D('',#11174,#5583,#5584);
#4747=AXIS2_PLACEMENT_3D('',#11176,#5585,#5586);
#4748=AXIS2_PLACEMENT_3D('',#11177,#5587,#5588);
#4749=AXIS2_PLACEMENT_3D('',#11178,#5589,#5590);
#4750=AXIS2_PLACEMENT_3D('',#11182,#5592,#5593);
#4751=AXIS2_PLACEMENT_3D('',#11184,#5595,#5596);
#4752=AXIS2_PLACEMENT_3D('',#11188,#5599,#5600);
#4753=AXIS2_PLACEMENT_3D('',#11192,#5603,#5604);
#4754=AXIS2_PLACEMENT_3D('',#11194,#5605,#5606);
#4755=AXIS2_PLACEMENT_3D('',#11197,#5608,#5609);
#4756=AXIS2_PLACEMENT_3D('',#11198,#5610,#5611);
#4757=AXIS2_PLACEMENT_3D('',#11200,#5612,#5613);
#4758=AXIS2_PLACEMENT_3D('',#11201,#5614,#5615);
#4759=AXIS2_PLACEMENT_3D('',#11202,#5616,#5617);
#4760=AXIS2_PLACEMENT_3D('',#11204,#5619,#5620);
#4761=AXIS2_PLACEMENT_3D('',#11206,#5621,#5622);
#4762=AXIS2_PLACEMENT_3D('',#11208,#5623,#5624);
#4763=AXIS2_PLACEMENT_3D('',#11209,#5625,#5626);
#4764=AXIS2_PLACEMENT_3D('',#11210,#5627,#5628);
#4765=AXIS2_PLACEMENT_3D('',#11212,#5629,#5630);
#4766=AXIS2_PLACEMENT_3D('',#11214,#5631,#5632);
#4767=AXIS2_PLACEMENT_3D('',#11216,#5633,#5634);
#4768=AXIS2_PLACEMENT_3D('',#11217,#5635,#5636);
#4769=AXIS2_PLACEMENT_3D('',#11218,#5637,#5638);
#4770=AXIS2_PLACEMENT_3D('',#11220,#5640,#5641);
#4771=AXIS2_PLACEMENT_3D('',#11224,#5643,#5644);
#4772=AXIS2_PLACEMENT_3D('',#11225,#5645,#5646);
#4773=AXIS2_PLACEMENT_3D('',#11226,#5647,#5648);
#4774=AXIS2_PLACEMENT_3D('',#11228,#5649,#5650);
#4775=AXIS2_PLACEMENT_3D('',#11229,#5651,#5652);
#4776=AXIS2_PLACEMENT_3D('',#11230,#5653,#5654);
#4777=AXIS2_PLACEMENT_3D('',#11232,#5656,#5657);
#4778=AXIS2_PLACEMENT_3D('',#11234,#5658,#5659);
#4779=AXIS2_PLACEMENT_3D('',#11237,#5662,#5663);
#4780=AXIS2_PLACEMENT_3D('',#11238,#5664,#5665);
#4781=AXIS2_PLACEMENT_3D('',#11239,#5666,#5667);
#4782=AXIS2_PLACEMENT_3D('',#11241,#5669,#5670);
#4783=AXIS2_PLACEMENT_3D('',#11242,#5671,#5672);
#4784=AXIS2_PLACEMENT_3D('',#11349,#5673,#5674);
#4785=AXIS2_PLACEMENT_3D('',#11372,#5675,#5676);
#4786=AXIS2_PLACEMENT_3D('',#11373,#5677,#5678);
#4787=AXIS2_PLACEMENT_3D('',#11376,#5680,#5681);
#4788=AXIS2_PLACEMENT_3D('',#11377,#5682,#5683);
#4789=AXIS2_PLACEMENT_3D('',#11378,#5684,#5685);
#4790=AXIS2_PLACEMENT_3D('',#11379,#5686,#5687);
#4791=AXIS2_PLACEMENT_3D('',#11380,#5688,#5689);
#4792=AXIS2_PLACEMENT_3D('',#11719,#5690,#5691);
#4793=AXIS2_PLACEMENT_3D('',#11751,#5693,#5694);
#4794=AXIS2_PLACEMENT_3D('',#11786,#5695,#5696);
#4795=AXIS2_PLACEMENT_3D('',#11787,#5697,#5698);
#4796=AXIS2_PLACEMENT_3D('',#11788,#5699,#5700);
#4797=AXIS2_PLACEMENT_3D('',#11789,#5701,#5702);
#4798=AXIS2_PLACEMENT_3D('',#11792,#5703,#5704);
#4799=AXIS2_PLACEMENT_3D('',#11793,#5705,#5706);
#4800=AXIS2_PLACEMENT_3D('',#11796,#5708,#5709);
#4801=AXIS2_PLACEMENT_3D('',#11797,#5710,#5711);
#4802=AXIS2_PLACEMENT_3D('',#11800,#5712,#5713);
#4803=AXIS2_PLACEMENT_3D('',#11801,#5714,#5715);
#4804=AXIS2_PLACEMENT_3D('',#11803,#5717,#5718);
#4805=AXIS2_PLACEMENT_3D('',#11805,#5719,#5720);
#4806=AXIS2_PLACEMENT_3D('',#11806,#5721,#5722);
#4807=AXIS2_PLACEMENT_3D('',#11808,#5723,#5724);
#4808=AXIS2_PLACEMENT_3D('',#11810,#5726,#5727);
#4809=AXIS2_PLACEMENT_3D('',#11812,#5728,#5729);
#4810=AXIS2_PLACEMENT_3D('',#11813,#5730,#5731);
#4811=AXIS2_PLACEMENT_3D('',#11818,#5733,#5734);
#4812=AXIS2_PLACEMENT_3D('',#11821,#5736,#5737);
#4813=AXIS2_PLACEMENT_3D('',#11822,#5738,#5739);
#4814=AXIS2_PLACEMENT_3D('',#11827,#5741,#5742);
#4815=AXIS2_PLACEMENT_3D('',#11830,#5744,#5745);
#4816=AXIS2_PLACEMENT_3D('',#11831,#5746,#5747);
#4817=AXIS2_PLACEMENT_3D('',#11835,#5750,#5751);
#4818=AXIS2_PLACEMENT_3D('',#11839,#5754,#5755);
#4819=AXIS2_PLACEMENT_3D('',#11843,#5758,#5759);
#4820=AXIS2_PLACEMENT_3D('',#11847,#5762,#5763);
#4821=AXIS2_PLACEMENT_3D('',#12130,#5770,#5771);
#4822=AXIS2_PLACEMENT_3D('',#12133,#5772,#5773);
#4823=AXIS2_PLACEMENT_3D('',#12134,#5774,#5775);
#4824=AXIS2_PLACEMENT_3D('',#12136,#5776,#5777);
#4825=AXIS2_PLACEMENT_3D('',#12138,#5778,#5779);
#4826=AXIS2_PLACEMENT_3D('',#12139,#5780,#5781);
#4827=AXIS2_PLACEMENT_3D('',#12140,#5782,#5783);
#4828=AXIS2_PLACEMENT_3D('',#12142,#5785,#5786);
#4829=AXIS2_PLACEMENT_3D('',#12145,#5787,#5788);
#4830=AXIS2_PLACEMENT_3D('',#12147,#5790,#5791);
#4831=AXIS2_PLACEMENT_3D('',#12148,#5792,#5793);
#4832=AXIS2_PLACEMENT_3D('',#12150,#5794,#5795);
#4833=AXIS2_PLACEMENT_3D('',#12152,#5796,#5797);
#4834=AXIS2_PLACEMENT_3D('',#12153,#5798,#5799);
#4835=AXIS2_PLACEMENT_3D('',#12154,#5800,#5801);
#4836=AXIS2_PLACEMENT_3D('',#12158,#5803,#5804);
#4837=AXIS2_PLACEMENT_3D('',#12160,#5806,#5807);
#4838=AXIS2_PLACEMENT_3D('',#12161,#5808,#5809);
#4839=AXIS2_PLACEMENT_3D('',#12199,#5810,#5811);
#4840=AXIS2_PLACEMENT_3D('',#12230,#5812,#5813);
#4841=AXIS2_PLACEMENT_3D('',#12237,#5814,#5815);
#4842=AXIS2_PLACEMENT_3D('',#12294,#5816,#5817);
#4843=AXIS2_PLACEMENT_3D('',#12420,#5818,#5819);
#4844=AXIS2_PLACEMENT_3D('',#12425,#5820,#5821);
#4845=AXIS2_PLACEMENT_3D('',#12427,#5822,#5823);
#4846=AXIS2_PLACEMENT_3D('',#12429,#5824,#5825);
#4847=AXIS2_PLACEMENT_3D('',#12430,#5826,#5827);
#4848=AXIS2_PLACEMENT_3D('',#12431,#5828,#5829);
#4849=AXIS2_PLACEMENT_3D('',#12432,#5830,#5831);
#4850=AXIS2_PLACEMENT_3D('',#12433,#5832,#5833);
#4851=AXIS2_PLACEMENT_3D('',#12434,#5834,#5835);
#4852=AXIS2_PLACEMENT_3D('',#12435,#5836,#5837);
#4853=AXIS2_PLACEMENT_3D('',#12449,#5843,#5844);
#4854=AXIS2_PLACEMENT_3D('',#12452,#5846,#5847);
#4855=AXIS2_PLACEMENT_3D('',#12453,#5848,#5849);
#4856=AXIS2_PLACEMENT_3D('',#12456,#5851,#5852);
#4857=AXIS2_PLACEMENT_3D('',#12457,#5853,#5854);
#4858=AXIS2_PLACEMENT_3D('',#12458,#5855,#5856);
#4859=AXIS2_PLACEMENT_3D('',#12459,#5857,#5858);
#4860=AXIS2_PLACEMENT_3D('',#12461,#5859,#5860);
#4861=AXIS2_PLACEMENT_3D('',#12462,#5861,#5862);
#4862=AXIS2_PLACEMENT_3D('',#12463,#5863,#5864);
#4863=AXIS2_PLACEMENT_3D('',#12465,#5865,#5866);
#4864=AXIS2_PLACEMENT_3D('',#12466,#5867,#5868);
#4865=AXIS2_PLACEMENT_3D('',#12469,#5869,#5870);
#4866=AXIS2_PLACEMENT_3D('',#12470,#5871,#5872);
#4867=AXIS2_PLACEMENT_3D('',#12471,#5873,#5874);
#4868=AXIS2_PLACEMENT_3D('',#12472,#5875,#5876);
#4869=AXIS2_PLACEMENT_3D('',#12476,#5878,#5879);
#4870=AXIS2_PLACEMENT_3D('',#12480,#5881,#5882);
#4871=AXIS2_PLACEMENT_3D('',#12483,#5884,#5885);
#4872=AXIS2_PLACEMENT_3D('',#12484,#5886,#5887);
#4873=AXIS2_PLACEMENT_3D('',#12486,#5889,#5890);
#4874=AXIS2_PLACEMENT_3D('',#12487,#5891,#5892);
#4875=AXIS2_PLACEMENT_3D('',#12488,#5893,#5894);
#4876=AXIS2_PLACEMENT_3D('',#12489,#5895,#5896);
#4877=AXIS2_PLACEMENT_3D('',#12490,#5897,#5898);
#4878=AXIS2_PLACEMENT_3D('',#12491,#5899,#5900);
#4879=AXIS2_PLACEMENT_3D('',#12492,#5901,#5902);
#4880=AXIS2_PLACEMENT_3D('',#12493,#5903,#5904);
#4881=AXIS2_PLACEMENT_3D('',#12504,#5905,#5906);
#4882=AXIS2_PLACEMENT_3D('',#12515,#5907,#5908);
#4883=AXIS2_PLACEMENT_3D('',#12516,#5909,#5910);
#4884=AXIS2_PLACEMENT_3D('',#12517,#5911,#5912);
#4885=AXIS2_PLACEMENT_3D('',#12518,#5913,#5914);
#4886=AXIS2_PLACEMENT_3D('',#12519,#5915,#5916);
#4887=AXIS2_PLACEMENT_3D('',#12521,#5917,#5918);
#4888=AXIS2_PLACEMENT_3D('',#12523,#5919,#5920);
#4889=AXIS2_PLACEMENT_3D('',#12525,#5921,#5922);
#4890=AXIS2_PLACEMENT_3D('',#12526,#5923,#5924);
#4891=AXIS2_PLACEMENT_3D('',#12527,#5925,#5926);
#4892=AXIS2_PLACEMENT_3D('',#12531,#5928,#5929);
#4893=AXIS2_PLACEMENT_3D('',#12532,#5930,#5931);
#4894=AXIS2_PLACEMENT_3D('',#12533,#5932,#5933);
#4895=AXIS2_PLACEMENT_3D('',#12535,#5934,#5935);
#4896=AXIS2_PLACEMENT_3D('',#12536,#5936,#5937);
#4897=AXIS2_PLACEMENT_3D('',#12538,#5938,#5939);
#4898=AXIS2_PLACEMENT_3D('',#12540,#5940,#5941);
#4899=AXIS2_PLACEMENT_3D('',#12541,#5942,#5943);
#4900=AXIS2_PLACEMENT_3D('',#12542,#5944,#5945);
#4901=AXIS2_PLACEMENT_3D('',#12546,#5947,#5948);
#4902=AXIS2_PLACEMENT_3D('',#12547,#5949,#5950);
#4903=AXIS2_PLACEMENT_3D('',#12548,#5951,#5952);
#4904=AXIS2_PLACEMENT_3D('',#12550,#5953,#5954);
#4905=AXIS2_PLACEMENT_3D('',#12551,#5955,#5956);
#4906=AXIS2_PLACEMENT_3D('',#12552,#5957,#5958);
#4907=AXIS2_PLACEMENT_3D('',#12554,#5959,#5960);
#4908=AXIS2_PLACEMENT_3D('',#12555,#5961,#5962);
#4909=AXIS2_PLACEMENT_3D('',#12557,#5963,#5964);
#4910=AXIS2_PLACEMENT_3D('',#12559,#5965,#5966);
#4911=AXIS2_PLACEMENT_3D('',#12560,#5967,#5968);
#4912=AXIS2_PLACEMENT_3D('',#12561,#5969,#5970);
#4913=AXIS2_PLACEMENT_3D('',#12564,#5971,#5972);
#4914=AXIS2_PLACEMENT_3D('',#12565,#5973,#5974);
#4915=AXIS2_PLACEMENT_3D('',#12567,#5976,#5977);
#4916=AXIS2_PLACEMENT_3D('',#12568,#5978,#5979);
#4917=AXIS2_PLACEMENT_3D('',#12569,#5980,#5981);
#4918=AXIS2_PLACEMENT_3D('',#12570,#5982,#5983);
#4919=AXIS2_PLACEMENT_3D('',#12572,#5984,#5985);
#4920=AXIS2_PLACEMENT_3D('',#12575,#5987,#5988);
#4921=AXIS2_PLACEMENT_3D('',#12576,#5989,#5990);
#4922=AXIS2_PLACEMENT_3D('',#12578,#5991,#5992);
#4923=AXIS2_PLACEMENT_3D('',#12579,#5993,#5994);
#4924=AXIS2_PLACEMENT_3D('',#12582,#5996,#5997);
#4925=AXIS2_PLACEMENT_3D('',#12583,#5998,#5999);
#4926=AXIS2_PLACEMENT_3D('',#12586,#6001,#6002);
#4927=AXIS2_PLACEMENT_3D('',#12587,#6003,#6004);
#4928=AXIS2_PLACEMENT_3D('',#12590,#6006,#6007);
#4929=AXIS2_PLACEMENT_3D('',#12591,#6008,#6009);
#4930=AXIS2_PLACEMENT_3D('',#12592,#6010,#6011);
#4931=AXIS2_PLACEMENT_3D('',#12593,#6012,#6013);
#4932=AXIS2_PLACEMENT_3D('',#12595,#6014,#6015);
#4933=AXIS2_PLACEMENT_3D('',#12598,#6017,#6018);
#4934=AXIS2_PLACEMENT_3D('',#12599,#6019,#6020);
#4935=AXIS2_PLACEMENT_3D('',#12601,#6021,#6022);
#4936=AXIS2_PLACEMENT_3D('',#12603,#6024,#6025);
#4937=AXIS2_PLACEMENT_3D('',#12605,#6026,#6027);
#4938=AXIS2_PLACEMENT_3D('',#12607,#6029,#6030);
#4939=AXIS2_PLACEMENT_3D('',#12609,#6031,#6032);
#4940=AXIS2_PLACEMENT_3D('',#12610,#6033,#6034);
#4941=AXIS2_PLACEMENT_3D('',#12613,#6036,#6037);
#4942=AXIS2_PLACEMENT_3D('',#12614,#6038,#6039);
#4943=AXIS2_PLACEMENT_3D('',#12615,#6040,#6041);
#4944=AXIS2_PLACEMENT_3D('',#12616,#6042,#6043);
#4945=AXIS2_PLACEMENT_3D('',#12618,#6044,#6045);
#4946=AXIS2_PLACEMENT_3D('',#12621,#6047,#6048);
#4947=AXIS2_PLACEMENT_3D('',#12622,#6049,#6050);
#4948=AXIS2_PLACEMENT_3D('',#12624,#6051,#6052);
#4949=AXIS2_PLACEMENT_3D('',#12627,#6054,#6055);
#4950=AXIS2_PLACEMENT_3D('',#12628,#6056,#6057);
#4951=AXIS2_PLACEMENT_3D('',#12637,#6061,#6062);
#4952=AXIS2_PLACEMENT_3D('',#12644,#6066,#6067);
#4953=AXIS2_PLACEMENT_3D('',#12645,#6068,#6069);
#4954=AXIS2_PLACEMENT_3D('',#12651,#6073,#6074);
#4955=AXIS2_PLACEMENT_3D('',#12655,#6077,#6078);
#4956=AXIS2_PLACEMENT_3D('',#12659,#6081,#6082);
#4957=AXIS2_PLACEMENT_3D('',#12663,#6084,#6085);
#4958=AXIS2_PLACEMENT_3D('',#12665,#6086,#6087);
#4959=AXIS2_PLACEMENT_3D('',#12669,#6090,#6091);
#4960=AXIS2_PLACEMENT_3D('',#12671,#6093,#6094);
#4961=AXIS2_PLACEMENT_3D('',#12673,#6096,#6097);
#4962=AXIS2_PLACEMENT_3D('',#12676,#6100,#6101);
#4963=AXIS2_PLACEMENT_3D('',#12677,#6102,#6103);
#4964=AXIS2_PLACEMENT_3D('',#12678,#6104,#6105);
#4965=AXIS2_PLACEMENT_3D('',#12679,#6106,#6107);
#4966=AXIS2_PLACEMENT_3D('',#12686,#6111,#6112);
#4967=AXIS2_PLACEMENT_3D('',#12693,#6116,#6117);
#4968=AXIS2_PLACEMENT_3D('',#12700,#6121,#6122);
#4969=AXIS2_PLACEMENT_3D('',#12707,#6126,#6127);
#4970=AXIS2_PLACEMENT_3D('',#12710,#6130,#6131);
#4971=AXIS2_PLACEMENT_3D('',#12717,#6135,#6136);
#4972=AXIS2_PLACEMENT_3D('',#12724,#6140,#6141);
#4973=AXIS2_PLACEMENT_3D('',#12727,#6144,#6145);
#4974=AXIS2_PLACEMENT_3D('',#12734,#6149,#6150);
#4975=AXIS2_PLACEMENT_3D('',#12737,#6153,#6154);
#4976=AXIS2_PLACEMENT_3D('',#12740,#6157,#6158);
#4977=AXIS2_PLACEMENT_3D('',#12747,#6162,#6163);
#4978=AXIS2_PLACEMENT_3D('',#12750,#6166,#6167);
#4979=AXIS2_PLACEMENT_3D('',#12753,#6170,#6171);
#4980=AXIS2_PLACEMENT_3D('',#12756,#6174,#6175);
#4981=AXIS2_PLACEMENT_3D('',#12759,#6178,#6179);
#4982=AXIS2_PLACEMENT_3D('',#12762,#6182,#6183);
#4983=AXIS2_PLACEMENT_3D('',#12765,#6186,#6187);
#4984=AXIS2_PLACEMENT_3D('',#12768,#6190,#6191);
#4985=AXIS2_PLACEMENT_3D('',#12771,#6194,#6195);
#4986=AXIS2_PLACEMENT_3D('',#12772,#6196,#6197);
#4987=AXIS2_PLACEMENT_3D('',#12773,#6198,#6199);
#4988=AXIS2_PLACEMENT_3D('',#12774,#6200,#6201);
#4989=AXIS2_PLACEMENT_3D('',#12775,#6202,#6203);
#4990=AXIS2_PLACEMENT_3D('',#12776,#6204,#6205);
#4991=AXIS2_PLACEMENT_3D('',#12777,#6206,#6207);
#4992=AXIS2_PLACEMENT_3D('',#12778,#6208,#6209);
#4993=AXIS2_PLACEMENT_3D('',#12779,#6210,#6211);
#4994=AXIS2_PLACEMENT_3D('',#12780,#6212,#6213);
#4995=AXIS2_PLACEMENT_3D('',#12781,#6214,#6215);
#4996=AXIS2_PLACEMENT_3D('',#12782,#6216,#6217);
#4997=AXIS2_PLACEMENT_3D('',#12783,#6218,#6219);
#4998=AXIS2_PLACEMENT_3D('',#12784,#6220,#6221);
#4999=AXIS2_PLACEMENT_3D('',#12785,#6222,#6223);
#5000=AXIS2_PLACEMENT_3D('',#12786,#6224,#6225);
#5001=AXIS2_PLACEMENT_3D('',#12787,#6226,#6227);
#5002=AXIS2_PLACEMENT_3D('',#12788,#6228,#6229);
#5003=AXIS2_PLACEMENT_3D('',#12789,#6230,#6231);
#5004=DIRECTION('axis',(0.,0.,1.));
#5005=DIRECTION('refdir',(1.,0.,0.));
#5006=DIRECTION('axis',(0.,0.,1.));
#5007=DIRECTION('refdir',(1.,0.,0.));
#5008=DIRECTION('center_axis',(1.,0.,0.));
#5009=DIRECTION('ref_axis',(0.,1.,0.));
#5010=DIRECTION('',(1.,0.,0.));
#5011=DIRECTION('center_axis',(-1.,0.,0.));
#5012=DIRECTION('ref_axis',(0.,1.,0.));
#5013=DIRECTION('center_axis',(-1.,0.,0.));
#5014=DIRECTION('ref_axis',(0.,1.,0.));
#5015=DIRECTION('center_axis',(1.48334715740448E-15,-5.5511151231258E-16,
1.));
#5016=DIRECTION('ref_axis',(-0.989545127054242,-0.144223581716739,1.38777878078145E-15));
#5017=DIRECTION('center_axis',(1.,0.,0.));
#5018=DIRECTION('ref_axis',(0.,0.,-1.));
#5019=DIRECTION('center_axis',(0.,-1.,-1.22464679914735E-16));
#5020=DIRECTION('ref_axis',(0.,-1.22464679914735E-16,1.));
#5021=DIRECTION('center_axis',(1.,0.,0.));
#5022=DIRECTION('ref_axis',(0.,-1.,1.83697019872103E-16));
#5023=DIRECTION('center_axis',(1.,0.,0.));
#5024=DIRECTION('ref_axis',(0.,0.,-1.));
#5025=DIRECTION('center_axis',(0.,1.03326339950577E-13,1.));
#5026=DIRECTION('ref_axis',(1.,0.,0.));
#5027=DIRECTION('center_axis',(0.,-3.49549273361196E-12,-1.));
#5028=DIRECTION('ref_axis',(-0.999873892461117,-0.0158807800392414,5.5511151231258E-14));
#5029=DIRECTION('center_axis',(1.,0.,0.));
#5030=DIRECTION('ref_axis',(0.,0.,-1.));
#5031=DIRECTION('center_axis',(1.,0.,0.));
#5032=DIRECTION('ref_axis',(0.,0.,-1.));
#5033=DIRECTION('center_axis',(1.,0.,0.));
#5034=DIRECTION('ref_axis',(0.,0.,-1.));
#5035=DIRECTION('center_axis',(0.,6.17228125957411E-12,1.));
#5036=DIRECTION('ref_axis',(-1.,0.,0.));
#5037=DIRECTION('center_axis',(-1.,0.,0.));
#5038=DIRECTION('ref_axis',(0.,0.,1.));
#5039=DIRECTION('center_axis',(1.,0.,0.));
#5040=DIRECTION('ref_axis',(0.,-1.,1.83697019872103E-16));
#5041=DIRECTION('center_axis',(1.,0.,0.));
#5042=DIRECTION('ref_axis',(0.,0.724568837309466,0.689202437604517));
#5043=DIRECTION('center_axis',(-1.,0.,0.));
#5044=DIRECTION('ref_axis',(0.,0.724568837309466,0.689202437604517));
#5045=DIRECTION('',(1.,0.,0.));
#5046=DIRECTION('center_axis',(-1.,0.,0.));
#5047=DIRECTION('ref_axis',(0.,0.,1.));
#5048=DIRECTION('',(-1.,0.,0.));
#5049=DIRECTION('center_axis',(0.,1.,0.));
#5050=DIRECTION('ref_axis',(0.,0.,1.));
#5051=DIRECTION('center_axis',(0.,-1.,0.));
#5052=DIRECTION('ref_axis',(0.707106781186553,0.,0.707106781186542));
#5053=DIRECTION('center_axis',(0.,1.,0.));
#5054=DIRECTION('ref_axis',(0.,0.,1.));
#5055=DIRECTION('',(0.,1.,0.));
#5056=DIRECTION('',(0.,-1.,0.));
#5057=DIRECTION('center_axis',(1.,0.,0.));
#5058=DIRECTION('ref_axis',(0.,0.,1.));
#5059=DIRECTION('center_axis',(-1.,0.,0.));
#5060=DIRECTION('ref_axis',(0.,-0.688576743024685,0.725163477407348));
#5061=DIRECTION('',(1.,0.,0.));
#5062=DIRECTION('',(-1.,0.,0.));
#5063=DIRECTION('center_axis',(0.,0.,-1.));
#5064=DIRECTION('ref_axis',(-1.,0.,0.));
#5065=DIRECTION('',(0.,1.,0.));
#5066=DIRECTION('center_axis',(1.,0.,0.));
#5067=DIRECTION('ref_axis',(0.,-0.688576743024685,-0.725163477407348));
#5068=DIRECTION('',(1.,0.,0.));
#5069=DIRECTION('center_axis',(-1.,0.,0.));
#5070=DIRECTION('ref_axis',(0.,0.,-1.));
#5071=DIRECTION('',(-1.,0.,0.));
#5072=DIRECTION('center_axis',(0.,-1.,0.));
#5073=DIRECTION('ref_axis',(0.,0.,-1.));
#5074=DIRECTION('center_axis',(0.,1.,0.));
#5075=DIRECTION('ref_axis',(0.707106781186553,0.,-0.707106781186542));
#5076=DIRECTION('center_axis',(0.,-1.,0.));
#5077=DIRECTION('ref_axis',(0.,0.,-1.));
#5078=DIRECTION('',(0.,-1.,0.));
#5079=DIRECTION('',(0.,1.,0.));
#5080=DIRECTION('center_axis',(1.,0.,0.));
#5081=DIRECTION('ref_axis',(0.,0.,-1.));
#5082=DIRECTION('center_axis',(-1.,0.,0.));
#5083=DIRECTION('ref_axis',(0.,0.724568837309466,-0.689202437604517));
#5084=DIRECTION('',(1.,0.,0.));
#5085=DIRECTION('',(-1.,0.,0.));
#5086=DIRECTION('center_axis',(-1.,0.,0.));
#5087=DIRECTION('ref_axis',(0.,0.724568837309466,-0.689202437604517));
#5088=DIRECTION('center_axis',(0.,0.,1.));
#5089=DIRECTION('ref_axis',(1.,0.,0.));
#5090=DIRECTION('',(0.,-1.,0.));
#5091=DIRECTION('center_axis',(-1.,0.,0.));
#5092=DIRECTION('ref_axis',(0.,0.,1.));
#5093=DIRECTION('center_axis',(1.,0.,0.));
#5094=DIRECTION('ref_axis',(0.,0.,1.));
#5095=DIRECTION('center_axis',(1.,0.,0.));
#5096=DIRECTION('ref_axis',(0.,1.,0.));
#5097=DIRECTION('center_axis',(-1.,0.,0.));
#5098=DIRECTION('ref_axis',(0.,-1.,0.));
#5099=DIRECTION('center_axis',(1.,0.,0.));
#5100=DIRECTION('ref_axis',(0.,1.,0.));
#5101=DIRECTION('center_axis',(1.,0.,0.));
#5102=DIRECTION('ref_axis',(0.,0.,-1.));
#5103=DIRECTION('center_axis',(1.,0.,0.));
#5104=DIRECTION('ref_axis',(0.,-1.,-1.22464679914735E-16));
#5105=DIRECTION('center_axis',(-1.,0.,0.));
#5106=DIRECTION('ref_axis',(0.,-1.,1.83697019872103E-16));
#5107=DIRECTION('center_axis',(1.,0.,0.));
#5108=DIRECTION('ref_axis',(0.,-1.,-6.12323399573677E-17));
#5109=DIRECTION('center_axis',(1.,0.,0.));
#5110=DIRECTION('ref_axis',(0.,-1.,1.83697019872103E-16));
#5111=DIRECTION('center_axis',(1.,0.,0.));
#5112=DIRECTION('ref_axis',(0.,0.,-1.));
#5113=DIRECTION('center_axis',(-1.,0.,0.));
#5114=DIRECTION('ref_axis',(0.,-1.,1.83697019872103E-16));
#5115=DIRECTION('center_axis',(1.,0.,0.));
#5116=DIRECTION('ref_axis',(0.,1.,0.));
#5117=DIRECTION('center_axis',(1.,0.,0.));
#5118=DIRECTION('ref_axis',(0.,-1.,1.83697019872103E-16));
#5119=DIRECTION('',(-1.,0.,0.));
#5120=DIRECTION('center_axis',(-1.,0.,0.));
#5121=DIRECTION('ref_axis',(0.,-1.,1.83697019872103E-16));
#5122=DIRECTION('center_axis',(-1.,0.,0.));
#5123=DIRECTION('ref_axis',(0.,-1.,1.83697019872103E-16));
#5124=DIRECTION('center_axis',(1.,0.,0.));
#5125=DIRECTION('ref_axis',(0.,-1.,1.83697019872103E-16));
#5126=DIRECTION('center_axis',(1.,0.,0.));
#5127=DIRECTION('ref_axis',(0.,-1.,-6.12323399573677E-17));
#5128=DIRECTION('center_axis',(1.,0.,0.));
#5129=DIRECTION('ref_axis',(0.,0.,-1.));
#5130=DIRECTION('center_axis',(0.,-1.,-1.22464679914735E-16));
#5131=DIRECTION('ref_axis',(0.,-1.22464679914735E-16,1.));
#5132=DIRECTION('axis',(0.,0.,1.));
#5133=DIRECTION('refdir',(1.,0.,0.));
#5134=DIRECTION('center_axis',(1.,0.,0.));
#5135=DIRECTION('ref_axis',(0.,0.,-1.));
#5136=DIRECTION('center_axis',(-1.,0.,0.));
#5137=DIRECTION('ref_axis',(0.,-1.,1.83697019872103E-16));
#5138=DIRECTION('center_axis',(0.,-1.,-1.22464679914735E-16));
#5139=DIRECTION('ref_axis',(0.,-1.22464679914735E-16,1.));
#5140=DIRECTION('center_axis',(1.,0.,0.));
#5141=DIRECTION('ref_axis',(0.,-1.,3.06161699786838E-17));
#5142=DIRECTION('center_axis',(1.,0.,0.));
#5143=DIRECTION('ref_axis',(0.,-1.,3.06161699786838E-17));
#5144=DIRECTION('center_axis',(-1.,0.,0.));
#5145=DIRECTION('ref_axis',(0.,1.,0.));
#5146=DIRECTION('',(-0.204863154122693,-0.978790625252869,-1.19867280625136E-16));
#5147=DIRECTION('center_axis',(-1.,0.,0.));
#5148=DIRECTION('ref_axis',(0.,-1.,3.06161699786838E-17));
#5149=DIRECTION('center_axis',(-1.,0.,0.));
#5150=DIRECTION('ref_axis',(0.,-1.,3.06161699786838E-17));
#5151=DIRECTION('center_axis',(1.,0.,0.));
#5152=DIRECTION('ref_axis',(0.,0.,-1.));
#5153=DIRECTION('center_axis',(1.,0.,0.));
#5154=DIRECTION('ref_axis',(0.,-1.,1.83697019872103E-16));
#5155=DIRECTION('center_axis',(1.,0.,0.));
#5156=DIRECTION('ref_axis',(0.,0.,-1.));
#5157=DIRECTION('center_axis',(0.,-1.,-1.22464679914735E-16));
#5158=DIRECTION('ref_axis',(0.,-1.22464679914735E-16,1.));
#5159=DIRECTION('center_axis',(1.,0.,0.));
#5160=DIRECTION('ref_axis',(0.,-1.,3.06161699786838E-17));
#5161=DIRECTION('center_axis',(1.,0.,0.));
#5162=DIRECTION('ref_axis',(0.,-1.,3.06161699786838E-17));
#5163=DIRECTION('center_axis',(-1.,0.,0.));
#5164=DIRECTION('ref_axis',(0.,1.,0.));
#5165=DIRECTION('',(-0.707106781186547,-0.707106781186547,-8.65956056235494E-17));
#5166=DIRECTION('center_axis',(-1.,0.,0.));
#5167=DIRECTION('ref_axis',(0.,-1.,3.06161699786838E-17));
#5168=DIRECTION('center_axis',(-1.,0.,0.));
#5169=DIRECTION('ref_axis',(0.,-1.,3.06161699786838E-17));
#5170=DIRECTION('center_axis',(1.,0.,0.));
#5171=DIRECTION('ref_axis',(0.,0.,-1.));
#5172=DIRECTION('center_axis',(0.,-1.,-1.22464679914735E-16));
#5173=DIRECTION('ref_axis',(0.,-1.22464679914735E-16,1.));
#5174=DIRECTION('center_axis',(1.,0.,0.));
#5175=DIRECTION('ref_axis',(0.,-1.,1.83697019872103E-16));
#5176=DIRECTION('center_axis',(1.,0.,0.));
#5177=DIRECTION('ref_axis',(0.,-1.,1.83697019872103E-16));
#5178=DIRECTION('center_axis',(1.,0.,0.));
#5179=DIRECTION('ref_axis',(0.,1.,0.));
#5180=DIRECTION('',(-1.,0.,0.));
#5181=DIRECTION('center_axis',(-1.,0.,0.));
#5182=DIRECTION('ref_axis',(0.,-1.,1.83697019872103E-16));
#5183=DIRECTION('center_axis',(-1.,0.,0.));
#5184=DIRECTION('ref_axis',(0.,-1.,1.83697019872103E-16));
#5185=DIRECTION('center_axis',(1.,0.,0.));
#5186=DIRECTION('ref_axis',(0.,0.,-1.));
#5187=DIRECTION('center_axis',(0.,-1.,-1.22464679914735E-16));
#5188=DIRECTION('ref_axis',(0.,-1.22464679914735E-16,1.));
#5189=DIRECTION('center_axis',(1.,0.,0.));
#5190=DIRECTION('ref_axis',(0.,-1.,3.06161699786838E-17));
#5191=DIRECTION('center_axis',(1.,0.,0.));
#5192=DIRECTION('ref_axis',(0.,-1.,3.06161699786838E-17));
#5193=DIRECTION('center_axis',(1.,0.,0.));
#5194=DIRECTION('ref_axis',(0.,1.,0.));
#5195=DIRECTION('',(-0.707106781186547,0.707106781186547,8.65956056235494E-17));
#5196=DIRECTION('center_axis',(-1.,0.,0.));
#5197=DIRECTION('ref_axis',(0.,-1.,3.06161699786838E-17));
#5198=DIRECTION('center_axis',(-1.,0.,0.));
#5199=DIRECTION('ref_axis',(0.,-1.,3.06161699786838E-17));
#5200=DIRECTION('center_axis',(1.,0.,0.));
#5201=DIRECTION('ref_axis',(0.,0.,-1.));
#5202=DIRECTION('center_axis',(0.,-1.,-1.22464679914735E-16));
#5203=DIRECTION('ref_axis',(0.,-1.22464679914735E-16,1.));
#5204=DIRECTION('center_axis',(1.,0.,0.));
#5205=DIRECTION('ref_axis',(0.,-1.,3.06161699786838E-17));
#5206=DIRECTION('center_axis',(1.,0.,0.));
#5207=DIRECTION('ref_axis',(0.,-1.,3.06161699786838E-17));
#5208=DIRECTION('center_axis',(1.,0.,0.));
#5209=DIRECTION('ref_axis',(0.,1.,0.));
#5210=DIRECTION('',(-0.174046612887447,0.984737415021084,1.20595552330621E-16));
#5211=DIRECTION('center_axis',(-1.,0.,0.));
#5212=DIRECTION('ref_axis',(0.,-1.,3.06161699786838E-17));
#5213=DIRECTION('center_axis',(-1.,0.,0.));
#5214=DIRECTION('ref_axis',(0.,-1.,3.06161699786838E-17));
#5215=DIRECTION('center_axis',(1.,0.,0.));
#5216=DIRECTION('ref_axis',(0.,0.,-1.));
#5217=DIRECTION('center_axis',(0.,-1.,-1.22464679914735E-16));
#5218=DIRECTION('ref_axis',(0.,-1.22464679914735E-16,1.));
#5219=DIRECTION('center_axis',(1.,0.,0.));
#5220=DIRECTION('ref_axis',(0.,-1.,1.83697019872103E-16));
#5221=DIRECTION('center_axis',(-1.,0.,0.));
#5222=DIRECTION('ref_axis',(0.,0.,1.));
#5223=DIRECTION('center_axis',(-1.,0.,0.));
#5224=DIRECTION('ref_axis',(0.,-1.,1.83697019872103E-16));
#5225=DIRECTION('center_axis',(1.,0.,0.));
#5226=DIRECTION('ref_axis',(0.,0.,-1.));
#5227=DIRECTION('center_axis',(0.,-1.,-1.22464679914735E-16));
#5228=DIRECTION('ref_axis',(0.,-1.22464679914735E-16,1.));
#5229=DIRECTION('center_axis',(1.,0.,0.));
#5230=DIRECTION('ref_axis',(0.,-1.,1.83697019872103E-16));
#5231=DIRECTION('center_axis',(1.,0.,0.));
#5232=DIRECTION('ref_axis',(0.,-1.,1.83697019872103E-16));
#5233=DIRECTION('center_axis',(1.,0.,0.));
#5234=DIRECTION('ref_axis',(0.,1.,0.));
#5235=DIRECTION('center_axis',(-1.,0.,0.));
#5236=DIRECTION('ref_axis',(0.,-1.,1.83697019872103E-16));
#5237=DIRECTION('center_axis',(-1.,0.,0.));
#5238=DIRECTION('ref_axis',(0.,-1.,1.83697019872103E-16));
#5239=DIRECTION('',(-1.,0.,0.));
#5240=DIRECTION('center_axis',(1.,0.,0.));
#5241=DIRECTION('ref_axis',(0.,0.,-1.));
#5242=DIRECTION('center_axis',(0.,-1.,-1.22464679914735E-16));
#5243=DIRECTION('ref_axis',(0.,-1.22464679914735E-16,1.));
#5244=DIRECTION('axis',(0.,0.,1.));
#5245=DIRECTION('refdir',(1.,0.,0.));
#5246=DIRECTION('center_axis',(1.,0.,0.));
#5247=DIRECTION('ref_axis',(0.,0.86829599907613,-0.496046427250903));
#5248=DIRECTION('',(1.,0.,0.));
#5249=DIRECTION('center_axis',(1.,0.,0.));
#5250=DIRECTION('ref_axis',(0.,1.,0.));
#5251=DIRECTION('center_axis',(1.,0.,0.));
#5252=DIRECTION('ref_axis',(0.,1.,0.));
#5253=DIRECTION('',(1.,0.,0.));
#5254=DIRECTION('center_axis',(1.,0.,0.));
#5255=DIRECTION('ref_axis',(0.,1.,0.));
#5256=DIRECTION('',(1.,0.,0.));
#5257=DIRECTION('center_axis',(1.,0.,0.));
#5258=DIRECTION('ref_axis',(0.,1.,0.));
#5259=DIRECTION('',(1.,0.,0.));
#5260=DIRECTION('center_axis',(1.,0.,0.));
#5261=DIRECTION('ref_axis',(0.,1.,0.));
#5262=DIRECTION('',(1.,0.,0.));
#5263=DIRECTION('center_axis',(1.,0.,0.));
#5264=DIRECTION('ref_axis',(0.,1.,0.));
#5265=DIRECTION('',(1.,0.,0.));
#5266=DIRECTION('center_axis',(1.,0.,0.));
#5267=DIRECTION('ref_axis',(0.,1.,0.));
#5268=DIRECTION('',(1.,0.,0.));
#5269=DIRECTION('center_axis',(1.,0.,0.));
#5270=DIRECTION('ref_axis',(0.,1.,0.));
#5271=DIRECTION('',(1.,0.,0.));
#5272=DIRECTION('center_axis',(1.,0.,0.));
#5273=DIRECTION('ref_axis',(0.,1.,0.));
#5274=DIRECTION('',(1.,0.,0.));
#5275=DIRECTION('center_axis',(1.,0.,0.));
#5276=DIRECTION('ref_axis',(0.,1.,0.));
#5277=DIRECTION('',(1.,0.,0.));
#5278=DIRECTION('center_axis',(1.,0.,0.));
#5279=DIRECTION('ref_axis',(0.,1.,0.));
#5280=DIRECTION('',(1.,0.,0.));
#5281=DIRECTION('center_axis',(1.,0.,0.));
#5282=DIRECTION('ref_axis',(0.,1.,0.));
#5283=DIRECTION('',(1.,0.,0.));
#5284=DIRECTION('center_axis',(1.,0.,0.));
#5285=DIRECTION('ref_axis',(0.,1.,0.));
#5286=DIRECTION('',(1.,0.,0.));
#5287=DIRECTION('center_axis',(1.,0.,0.));
#5288=DIRECTION('ref_axis',(0.,1.,0.));
#5289=DIRECTION('',(1.,0.,0.));
#5290=DIRECTION('center_axis',(1.,0.,0.));
#5291=DIRECTION('ref_axis',(0.,1.,0.));
#5292=DIRECTION('',(1.,0.,0.));
#5293=DIRECTION('center_axis',(1.,0.,0.));
#5294=DIRECTION('ref_axis',(0.,1.,0.));
#5295=DIRECTION('',(1.,0.,0.));
#5296=DIRECTION('center_axis',(1.,0.,0.));
#5297=DIRECTION('ref_axis',(0.,0.941324933064923,0.337501659833428));
#5298=DIRECTION('',(1.,0.,0.));
#5299=DIRECTION('center_axis',(1.,0.,0.));
#5300=DIRECTION('ref_axis',(0.,1.,0.));
#5301=DIRECTION('center_axis',(1.,0.,0.));
#5302=DIRECTION('ref_axis',(0.,-0.654392380830797,-0.75615515068708));
#5303=DIRECTION('',(1.,1.22464679914735E-16,1.26773667528936E-29));
#5304=DIRECTION('center_axis',(-1.,0.,0.));
#5305=DIRECTION('ref_axis',(0.,1.,1.03396090724959E-13));
#5306=DIRECTION('center_axis',(1.,0.,0.));
#5307=DIRECTION('ref_axis',(0.,1.,1.03396090724959E-13));
#5308=DIRECTION('',(1.,1.22464679914735E-16,1.26773667528936E-29));
#5309=DIRECTION('center_axis',(1.,0.,0.));
#5310=DIRECTION('ref_axis',(0.,1.,1.03396090724959E-13));
#5311=DIRECTION('',(1.,1.22464679914735E-16,1.26773667528936E-29));
#5312=DIRECTION('center_axis',(1.,0.,0.));
#5313=DIRECTION('ref_axis',(0.,1.,1.03396090724959E-13));
#5314=DIRECTION('',(1.,1.22464679914735E-16,1.26773667528936E-29));
#5315=DIRECTION('center_axis',(1.,0.,0.));
#5316=DIRECTION('ref_axis',(0.,1.,1.03396090724959E-13));
#5317=DIRECTION('',(1.,1.22464679914735E-16,1.26773667528936E-29));
#5318=DIRECTION('center_axis',(1.,0.,0.));
#5319=DIRECTION('ref_axis',(0.,1.,1.03396090724959E-13));
#5320=DIRECTION('',(1.,1.22464679914735E-16,1.26773667528936E-29));
#5321=DIRECTION('center_axis',(1.,0.,0.));
#5322=DIRECTION('ref_axis',(0.,1.,1.03396090724959E-13));
#5323=DIRECTION('',(1.,1.22464679914735E-16,1.26773667528936E-29));
#5324=DIRECTION('center_axis',(1.,0.,0.));
#5325=DIRECTION('ref_axis',(0.,1.,1.03396090724959E-13));
#5326=DIRECTION('',(1.,1.22464679914735E-16,1.26773667528936E-29));
#5327=DIRECTION('center_axis',(1.,0.,0.));
#5328=DIRECTION('ref_axis',(0.,1.,1.03396090724959E-13));
#5329=DIRECTION('',(1.,1.22464679914735E-16,1.26773667528936E-29));
#5330=DIRECTION('center_axis',(1.,0.,0.));
#5331=DIRECTION('ref_axis',(0.,1.,1.03396090724959E-13));
#5332=DIRECTION('',(1.,1.22464679914735E-16,1.26773667528936E-29));
#5333=DIRECTION('center_axis',(1.,0.,0.));
#5334=DIRECTION('ref_axis',(0.,1.,1.03396090724959E-13));
#5335=DIRECTION('',(1.,1.22464679914735E-16,1.26773667528936E-29));
#5336=DIRECTION('center_axis',(1.,0.,0.));
#5337=DIRECTION('ref_axis',(0.,1.,1.03396090724959E-13));
#5338=DIRECTION('',(1.,1.22464679914735E-16,1.26773667528936E-29));
#5339=DIRECTION('center_axis',(1.,0.,0.));
#5340=DIRECTION('ref_axis',(0.,1.,1.03396090724959E-13));
#5341=DIRECTION('',(1.,1.22464679914735E-16,1.26773667528936E-29));
#5342=DIRECTION('center_axis',(1.,0.,0.));
#5343=DIRECTION('ref_axis',(0.,1.,1.03396090724959E-13));
#5344=DIRECTION('',(1.,1.22464679914735E-16,1.26773667528936E-29));
#5345=DIRECTION('center_axis',(1.,0.,0.));
#5346=DIRECTION('ref_axis',(0.,1.,1.03396090724959E-13));
#5347=DIRECTION('',(1.,1.22464679914735E-16,1.26773667528936E-29));
#5348=DIRECTION('center_axis',(1.,0.,0.));
#5349=DIRECTION('ref_axis',(0.,1.,1.03396090724959E-13));
#5350=DIRECTION('',(1.,1.22464679914735E-16,1.26773667528936E-29));
#5351=DIRECTION('center_axis',(1.,0.,0.));
#5352=DIRECTION('ref_axis',(0.,1.,1.03396090724959E-13));
#5353=DIRECTION('',(1.,1.22464679914735E-16,1.26773667528936E-29));
#5354=DIRECTION('center_axis',(1.,0.,0.));
#5355=DIRECTION('ref_axis',(0.,-0.512398366081367,0.85874787594331));
#5356=DIRECTION('',(1.,1.22464679914735E-16,1.26773667528936E-29));
#5357=DIRECTION('center_axis',(1.,0.,0.));
#5358=DIRECTION('ref_axis',(0.,1.,1.03396090724959E-13));
#5359=DIRECTION('center_axis',(1.,0.,0.));
#5360=DIRECTION('ref_axis',(0.,0.,-1.));
#5361=DIRECTION('center_axis',(1.,0.,0.));
#5362=DIRECTION('ref_axis',(0.,1.,0.));
#5363=DIRECTION('center_axis',(1.,0.,0.));
#5364=DIRECTION('ref_axis',(0.,1.,0.));
#5365=DIRECTION('center_axis',(1.,0.,0.));
#5366=DIRECTION('ref_axis',(0.,1.,1.03396090724959E-13));
#5367=DIRECTION('center_axis',(1.,0.,0.));
#5368=DIRECTION('ref_axis',(0.,0.,-1.));
#5369=DIRECTION('center_axis',(1.,0.,0.));
#5370=DIRECTION('ref_axis',(0.,1.,0.));
#5371=DIRECTION('center_axis',(1.,0.,0.));
#5372=DIRECTION('ref_axis',(0.,1.,0.));
#5373=DIRECTION('center_axis',(1.,0.,0.));
#5374=DIRECTION('ref_axis',(0.,1.,0.));
#5375=DIRECTION('',(0.515038074910053,-0.857167300702113,-1.04972719113862E-16));
#5376=DIRECTION('center_axis',(1.,0.,0.));
#5377=DIRECTION('ref_axis',(0.,1.,0.));
#5378=DIRECTION('center_axis',(1.,0.,0.));
#5379=DIRECTION('ref_axis',(0.,1.,0.));
#5380=DIRECTION('',(0.70710678118654,-0.707106781186555,-8.65956056235502E-17));
#5381=DIRECTION('center_axis',(-1.,0.,0.));
#5382=DIRECTION('ref_axis',(0.,1.,0.));
#5383=DIRECTION('center_axis',(0.,0.,1.));
#5384=DIRECTION('ref_axis',(1.,0.,0.));
#5385=DIRECTION('',(-1.,0.,0.));
#5386=DIRECTION('',(0.,1.,0.));
#5387=DIRECTION('',(1.,0.,0.));
#5388=DIRECTION('',(0.,-1.,0.));
#5389=DIRECTION('center_axis',(-1.,0.,0.));
#5390=DIRECTION('ref_axis',(0.,-1.,0.));
#5391=DIRECTION('center_axis',(-1.,0.,0.));
#5392=DIRECTION('ref_axis',(0.,1.,0.));
#5393=DIRECTION('',(0.,0.,1.));
#5394=DIRECTION('',(0.,1.,0.));
#5395=DIRECTION('center_axis',(0.,0.,-1.));
#5396=DIRECTION('ref_axis',(-1.,0.,0.));
#5397=DIRECTION('',(1.,0.,0.));
#5398=DIRECTION('',(-1.,0.,0.));
#5399=DIRECTION('',(0.,-1.,0.));
#5400=DIRECTION('center_axis',(1.,0.,0.));
#5401=DIRECTION('ref_axis',(0.,1.,0.));
#5402=DIRECTION('center_axis',(1.,0.,0.));
#5403=DIRECTION('ref_axis',(0.,1.,0.));
#5404=DIRECTION('',(0.,0.,1.));
#5405=DIRECTION('center_axis',(0.,-1.,0.));
#5406=DIRECTION('ref_axis',(1.,0.,0.));
#5407=DIRECTION('center_axis',(0.,0.,1.));
#5408=DIRECTION('ref_axis',(1.,0.,0.));
#5409=DIRECTION('',(-1.,0.,0.));
#5410=DIRECTION('',(0.,1.,0.));
#5411=DIRECTION('',(1.,0.,0.));
#5412=DIRECTION('',(0.,-1.,0.));
#5413=DIRECTION('center_axis',(-1.,0.,0.));
#5414=DIRECTION('ref_axis',(0.,-1.,0.));
#5415=DIRECTION('center_axis',(-1.,0.,0.));
#5416=DIRECTION('ref_axis',(0.,1.,0.));
#5417=DIRECTION('',(0.,0.,1.));
#5418=DIRECTION('',(0.,1.,0.));
#5419=DIRECTION('center_axis',(0.,0.,-1.));
#5420=DIRECTION('ref_axis',(-1.,0.,0.));
#5421=DIRECTION('',(1.,0.,0.));
#5422=DIRECTION('',(-1.,0.,0.));
#5423=DIRECTION('',(0.,-1.,0.));
#5424=DIRECTION('center_axis',(1.,0.,0.));
#5425=DIRECTION('ref_axis',(0.,1.,0.));
#5426=DIRECTION('center_axis',(1.,0.,0.));
#5427=DIRECTION('ref_axis',(0.,1.,0.));
#5428=DIRECTION('',(0.,0.,1.));
#5429=DIRECTION('center_axis',(0.,-1.,0.));
#5430=DIRECTION('ref_axis',(1.,0.,0.));
#5431=DIRECTION('center_axis',(1.,0.,0.));
#5432=DIRECTION('ref_axis',(0.,0.,-1.));
#5433=DIRECTION('center_axis',(1.,0.,0.));
#5434=DIRECTION('ref_axis',(0.,1.,0.));
#5435=DIRECTION('center_axis',(1.,0.,0.));
#5436=DIRECTION('ref_axis',(0.,0.,-1.));
#5437=DIRECTION('center_axis',(1.,0.,0.));
#5438=DIRECTION('ref_axis',(0.,1.,0.));
#5439=DIRECTION('center_axis',(1.,0.,0.));
#5440=DIRECTION('ref_axis',(0.,0.,-1.));
#5441=DIRECTION('',(1.,0.,0.));
#5442=DIRECTION('center_axis',(-1.,0.,0.));
#5443=DIRECTION('ref_axis',(0.,0.,1.));
#5444=DIRECTION('center_axis',(-1.,0.,0.));
#5445=DIRECTION('ref_axis',(0.,1.,0.));
#5446=DIRECTION('center_axis',(1.,0.,0.));
#5447=DIRECTION('ref_axis',(0.,1.,0.));
#5448=DIRECTION('',(-1.,0.,0.));
#5449=DIRECTION('center_axis',(1.,0.,0.));
#5450=DIRECTION('ref_axis',(0.,1.,0.));
#5451=DIRECTION('center_axis',(1.,0.,0.));
#5452=DIRECTION('ref_axis',(0.,0.,-1.));
#5453=DIRECTION('center_axis',(1.,0.,0.));
#5454=DIRECTION('ref_axis',(0.,0.,-1.));
#5455=DIRECTION('center_axis',(1.,0.,0.));
#5456=DIRECTION('ref_axis',(0.,1.,0.));
#5457=DIRECTION('center_axis',(1.,0.,0.));
#5458=DIRECTION('ref_axis',(0.,0.,-1.));
#5459=DIRECTION('',(1.,0.,0.));
#5460=DIRECTION('center_axis',(-1.,0.,0.));
#5461=DIRECTION('ref_axis',(0.,0.,1.));
#5462=DIRECTION('center_axis',(-1.,0.,0.));
#5463=DIRECTION('ref_axis',(0.,1.,0.));
#5464=DIRECTION('center_axis',(1.,0.,0.));
#5465=DIRECTION('ref_axis',(0.,1.,0.));
#5466=DIRECTION('',(-1.,0.,0.));
#5467=DIRECTION('center_axis',(1.,0.,0.));
#5468=DIRECTION('ref_axis',(0.,0.,-1.));
#5469=DIRECTION('center_axis',(-1.,0.,0.));
#5470=DIRECTION('ref_axis',(0.,0.,1.));
#5471=DIRECTION('center_axis',(1.,0.,0.));
#5472=DIRECTION('ref_axis',(0.,0.,-1.));
#5473=DIRECTION('center_axis',(1.,0.,0.));
#5474=DIRECTION('ref_axis',(0.,1.,0.));
#5475=DIRECTION('',(-0.707106781186547,0.707106781186548,8.65956056235494E-17));
#5476=DIRECTION('center_axis',(1.,0.,0.));
#5477=DIRECTION('ref_axis',(0.,1.,0.));
#5478=DIRECTION('center_axis',(1.,0.,0.));
#5479=DIRECTION('ref_axis',(0.,0.,-1.));
#5480=DIRECTION('',(-1.,0.,0.));
#5481=DIRECTION('center_axis',(-1.,0.,0.));
#5482=DIRECTION('ref_axis',(0.,1.,0.));
#5483=DIRECTION('center_axis',(1.,0.,0.));
#5484=DIRECTION('ref_axis',(0.,0.,-1.));
#5485=DIRECTION('',(-0.707106781186556,-0.707106781186539,-8.65956056235483E-17));
#5486=DIRECTION('center_axis',(1.,0.,0.));
#5487=DIRECTION('ref_axis',(0.,0.,-1.));
#5488=DIRECTION('axis',(0.,0.,1.));
#5489=DIRECTION('refdir',(1.,0.,0.));
#5490=DIRECTION('center_axis',(1.,0.,0.));
#5491=DIRECTION('ref_axis',(0.,-1.,1.83697019872103E-16));
#5492=DIRECTION('center_axis',(-1.5851531306331E-14,-0.044221029995557,
0.999021771787849));
#5493=DIRECTION('ref_axis',(-1.,-1.77635683940025E-14,-1.66533453693773E-14));
#5494=DIRECTION('center_axis',(1.,0.,0.));
#5495=DIRECTION('ref_axis',(0.,-1.,3.06161699786838E-17));
#5496=DIRECTION('center_axis',(2.43686520408589E-13,-0.0442210299954363,
-0.999021771787854));
#5497=DIRECTION('ref_axis',(-0.640184399668964,-0.767469783864776,0.0339715362478869));
#5498=DIRECTION('center_axis',(-1.,0.,0.));
#5499=DIRECTION('ref_axis',(0.,-1.,1.83697019872103E-16));
#5500=DIRECTION('center_axis',(-0.449113375415322,-0.210147679264594,-0.868409539861673));
#5501=DIRECTION('ref_axis',(-0.786560864598894,-0.368045017904336,0.495847628891413));
#5502=DIRECTION('center_axis',(0.,-1.,0.));
#5503=DIRECTION('ref_axis',(-0.707106781186548,0.,0.707106781186547));
#5504=DIRECTION('center_axis',(0.449113375415322,0.210147679264594,-0.868409539861672));
#5505=DIRECTION('ref_axis',(-0.786560864598894,-0.368045017904336,-0.495847628891415));
#5506=DIRECTION('center_axis',(0.,-1.,0.));
#5507=DIRECTION('ref_axis',(-0.707106781186548,0.,-0.707106781186547));
#5508=DIRECTION('center_axis',(0.767910450456811,-0.640557210621517,-3.00737669654705E-13));
#5509=DIRECTION('ref_axis',(-0.640184399664482,-0.76746351858997,-0.0341127844030622));
#5510=DIRECTION('center_axis',(0.,-1.,0.));
#5511=DIRECTION('ref_axis',(-0.707106781186548,0.,-0.707106781186547));
#5512=DIRECTION('',(0.,1.,0.));
#5513=DIRECTION('center_axis',(0.,-1.,0.));
#5514=DIRECTION('ref_axis',(-1.,0.,0.));
#5515=DIRECTION('',(0.,-1.,0.));
#5516=DIRECTION('center_axis',(-1.,0.,0.));
#5517=DIRECTION('ref_axis',(0.,0.,1.));
#5518=DIRECTION('',(0.,-1.,0.));
#5519=DIRECTION('center_axis',(6.37222258072231E-14,-0.0444048938881032,
-0.999013616222915));
#5520=DIRECTION('ref_axis',(-0.0166242555004783,-0.998875560049686,0.0443987574655116));
#5521=DIRECTION('center_axis',(2.56046860681907E-14,-0.0444048938880752,
0.999013616222917));
#5522=DIRECTION('ref_axis',(-0.640184399664478,-0.767463518589973,-0.0341127844030666));
#5523=DIRECTION('center_axis',(-0.953150734475215,0.258173802549692,-0.157638716838187));
#5524=DIRECTION('ref_axis',(-0.302495747688061,-0.813494243814166,0.496712631117691));
#5525=DIRECTION('center_axis',(-0.999861534547107,0.0166406650439521,0.));
#5526=DIRECTION('ref_axis',(-1.68476343986872E-13,3.5527136788006E-14,1.));
#5527=DIRECTION('center_axis',(0.76791045045681,-0.640557210621518,1.08864901799987E-13));
#5528=DIRECTION('ref_axis',(-1.68476343986872E-13,3.5527136788006E-14,1.));
#5529=DIRECTION('center_axis',(-0.953150734475031,0.258173802550189,0.15763871683849));
#5530=DIRECTION('ref_axis',(-0.302495747688635,-0.813494243814005,-0.496712631117605));
#5531=DIRECTION('center_axis',(-0.999861534547107,0.0166406650439596,0.));
#5532=DIRECTION('ref_axis',(-3.95794508278868E-13,-1.77635683940025E-14,
-1.));
#5533=DIRECTION('center_axis',(0.,0.,1.));
#5534=DIRECTION('ref_axis',(1.,0.,0.));
#5535=DIRECTION('',(0.,1.,0.));
#5536=DIRECTION('center_axis',(-7.51780949620696E-14,3.98534670278357E-13,
1.));
#5537=DIRECTION('ref_axis',(-0.987805559694749,-0.155692569624061,-1.22124532708767E-14));
#5538=DIRECTION('center_axis',(-1.,0.,0.));
#5539=DIRECTION('ref_axis',(0.,1.,0.));
#5540=DIRECTION('center_axis',(1.,0.,0.));
#5541=DIRECTION('ref_axis',(0.,0.,-1.));
#5542=DIRECTION('',(-0.196116135138184,-0.98058067569092,-1.20086498579063E-16));
#5543=DIRECTION('center_axis',(1.,0.,0.));
#5544=DIRECTION('ref_axis',(0.,0.,-1.));
#5545=DIRECTION('center_axis',(-1.,0.,0.));
#5546=DIRECTION('ref_axis',(0.,-1.,1.83697019872103E-16));
#5547=DIRECTION('center_axis',(-1.,0.,0.));
#5548=DIRECTION('ref_axis',(0.,-1.,1.83697019872103E-16));
#5549=DIRECTION('center_axis',(0.,-1.,-1.22464679914735E-16));
#5550=DIRECTION('ref_axis',(0.,-1.22464679914735E-16,1.));
#5551=DIRECTION('center_axis',(1.,0.,0.));
#5552=DIRECTION('ref_axis',(0.,-1.,1.83697019872103E-16));
#5553=DIRECTION('center_axis',(-1.,0.,0.));
#5554=DIRECTION('ref_axis',(0.,0.,1.));
#5555=DIRECTION('',(0.,1.,0.));
#5556=DIRECTION('center_axis',(-1.,0.,0.));
#5557=DIRECTION('ref_axis',(0.,-1.,1.83697019872103E-16));
#5558=DIRECTION('',(0.,-1.,0.));
#5559=DIRECTION('',(0.,0.,-1.));
#5560=DIRECTION('center_axis',(1.,0.,0.));
#5561=DIRECTION('ref_axis',(0.,1.,0.));
#5562=DIRECTION('center_axis',(1.,0.,0.));
#5563=DIRECTION('ref_axis',(0.,0.,-1.));
#5564=DIRECTION('',(-1.,0.,0.));
#5565=DIRECTION('center_axis',(0.,0.,1.));
#5566=DIRECTION('ref_axis',(-0.707106781186546,-0.707106781186549,0.));
#5567=DIRECTION('center_axis',(0.,-0.707106781186547,-0.707106781186548));
#5568=DIRECTION('ref_axis',(0.,-0.707106781186548,0.707106781186547));
#5569=DIRECTION('',(0.,0.,1.));
#5570=DIRECTION('center_axis',(0.,0.707106781186547,-0.707106781186548));
#5571=DIRECTION('ref_axis',(0.,-0.707106781186548,-0.707106781186547));
#5572=DIRECTION('center_axis',(0.,-1.,0.));
#5573=DIRECTION('ref_axis',(-0.707106781186548,0.,-0.707106781186547));
#5574=DIRECTION('',(0.,-1.,0.));
#5575=DIRECTION('center_axis',(0.,1.,0.));
#5576=DIRECTION('ref_axis',(0.,0.,-1.));
#5577=DIRECTION('center_axis',(0.288199153586547,-0.87432067514108,0.390518379711947));
#5578=DIRECTION('ref_axis',(-0.519169991490067,-0.485348696321363,-0.70349069852796));
#5579=DIRECTION('center_axis',(-1.,0.,0.));
#5580=DIRECTION('ref_axis',(0.,-0.567877810008977,-0.823112867655104));
#5581=DIRECTION('center_axis',(0.,0.355029585798816,-0.934855065348378));
#5582=DIRECTION('ref_axis',(0.,0.934855065348378,0.355029585798816));
#5583=DIRECTION('center_axis',(1.,0.,0.));
#5584=DIRECTION('ref_axis',(0.,-1.,1.83697019872103E-16));
#5585=DIRECTION('center_axis',(1.,0.,0.));
#5586=DIRECTION('ref_axis',(0.,-1.,1.83697019872103E-16));
#5587=DIRECTION('center_axis',(0.,0.355029585798817,0.934855065348378));
#5588=DIRECTION('ref_axis',(0.,-0.934855065348378,0.355029585798817));
#5589=DIRECTION('center_axis',(1.,0.,0.));
#5590=DIRECTION('ref_axis',(0.,-0.567877810008977,-0.823112867655104));
#5591=DIRECTION('',(1.,0.,0.));
#5592=DIRECTION('center_axis',(1.,0.,0.));
#5593=DIRECTION('ref_axis',(0.,-0.567877810008977,-0.823112867655104));
#5594=DIRECTION('',(-1.,0.,0.));
#5595=DIRECTION('center_axis',(0.,0.,1.));
#5596=DIRECTION('ref_axis',(1.,0.,0.));
#5597=DIRECTION('',(-1.,0.,0.));
#5598=DIRECTION('',(0.,1.,0.));
#5599=DIRECTION('center_axis',(0.,1.,0.));
#5600=DIRECTION('ref_axis',(-1.,0.,0.));
#5601=DIRECTION('',(1.,0.,0.));
#5602=DIRECTION('',(0.,0.,-1.));
#5603=DIRECTION('center_axis',(0.,0.,-1.));
#5604=DIRECTION('ref_axis',(0.707106781186544,-0.707106781186551,0.));
#5605=DIRECTION('center_axis',(0.,-0.707106781186549,-0.707106781186546));
#5606=DIRECTION('ref_axis',(-4.90653893338679E-17,-0.707106781186546,0.707106781186549));
#5607=DIRECTION('',(0.,0.,1.));
#5608=DIRECTION('center_axis',(0.,0.707106781186547,-0.707106781186548));
#5609=DIRECTION('ref_axis',(0.,0.707106781186548,0.707106781186547));
#5610=DIRECTION('center_axis',(-0.288199153586547,-0.87432067514108,0.390518379711947));
#5611=DIRECTION('ref_axis',(0.519169991490067,-0.485348696321362,-0.703490698527961));
#5612=DIRECTION('center_axis',(0.,-1.,-2.22044604925031E-15));
#5613=DIRECTION('ref_axis',(0.,2.22044604925031E-15,-1.));
#5614=DIRECTION('center_axis',(0.,0.355029585798817,-0.934855065348378));
#5615=DIRECTION('ref_axis',(0.,0.934855065348378,0.355029585798817));
#5616=DIRECTION('center_axis',(0.,1.,0.));
#5617=DIRECTION('ref_axis',(0.707106781186547,0.,-0.707106781186548));
#5618=DIRECTION('',(0.,-1.,0.));
#5619=DIRECTION('center_axis',(1.,0.,0.));
#5620=DIRECTION('ref_axis',(0.,-1.,1.83697019872103E-16));
#5621=DIRECTION('center_axis',(1.,0.,0.));
#5622=DIRECTION('ref_axis',(0.,-0.999438109969484,0.0335181195866625));
#5623=DIRECTION('center_axis',(1.28747119532049E-15,-0.355029585798816,
-0.934855065348379));
#5624=DIRECTION('ref_axis',(1.,-2.22044604925031E-15,2.22044604925031E-15));
#5625=DIRECTION('center_axis',(-1.,0.,0.));
#5626=DIRECTION('ref_axis',(0.,-0.999438109969484,0.0335181195866626));
#5627=DIRECTION('center_axis',(1.,0.,0.));
#5628=DIRECTION('ref_axis',(0.,0.,-1.));
#5629=DIRECTION('center_axis',(-1.,0.,0.));
#5630=DIRECTION('ref_axis',(0.,-1.,1.83697019872103E-16));
#5631=DIRECTION('center_axis',(0.,-1.,-1.22464679914735E-16));
#5632=DIRECTION('ref_axis',(0.,-1.22464679914735E-16,1.));
#5633=DIRECTION('center_axis',(1.,0.,0.));
#5634=DIRECTION('ref_axis',(0.,-1.,3.06161699786838E-17));
#5635=DIRECTION('center_axis',(1.,0.,0.));
#5636=DIRECTION('ref_axis',(0.,-1.,3.06161699786838E-17));
#5637=DIRECTION('center_axis',(1.,0.,0.));
#5638=DIRECTION('ref_axis',(0.,0.,-1.));
#5639=DIRECTION('',(0.,1.,0.));
#5640=DIRECTION('center_axis',(-1.,0.,0.));
#5641=DIRECTION('ref_axis',(0.,1.,0.));
#5642=DIRECTION('',(-0.171609399198264,-0.985165069471513,-1.20647924896007E-16));
#5643=DIRECTION('center_axis',(1.,0.,0.));
#5644=DIRECTION('ref_axis',(0.,0.,-1.));
#5645=DIRECTION('center_axis',(1.,0.,0.));
#5646=DIRECTION('ref_axis',(0.,0.,-1.));
#5647=DIRECTION('center_axis',(0.288199153586548,-0.874320675141079,-0.390518379711948));
#5648=DIRECTION('ref_axis',(-0.519169991490068,-0.485348696321364,0.703490698527959));
#5649=DIRECTION('center_axis',(-1.,0.,0.));
#5650=DIRECTION('ref_axis',(0.,0.,1.));
#5651=DIRECTION('center_axis',(0.,-1.,0.));
#5652=DIRECTION('ref_axis',(-1.,0.,0.));
#5653=DIRECTION('center_axis',(0.,1.,0.));
#5654=DIRECTION('ref_axis',(-0.707106781186548,0.,0.707106781186547));
#5655=DIRECTION('',(0.,1.,0.));
#5656=DIRECTION('center_axis',(-1.,0.,0.));
#5657=DIRECTION('ref_axis',(0.,-0.567877810008977,0.823112867655104));
#5658=DIRECTION('center_axis',(-1.,0.,0.));
#5659=DIRECTION('ref_axis',(0.,-0.934855065348378,0.355029585798817));
#5660=DIRECTION('',(-1.,0.,0.));
#5661=DIRECTION('',(1.,0.,0.));
#5662=DIRECTION('center_axis',(-0.288199153586547,-0.87432067514108,-0.390518379711947));
#5663=DIRECTION('ref_axis',(0.519169991490067,-0.485348696321363,0.70349069852796));
#5664=DIRECTION('center_axis',(0.,-1.,0.));
#5665=DIRECTION('ref_axis',(0.707106781186546,0.,0.707106781186549));
#5666=DIRECTION('center_axis',(0.,0.,-1.));
#5667=DIRECTION('ref_axis',(-1.,0.,0.));
#5668=DIRECTION('',(0.,-1.,0.));
#5669=DIRECTION('center_axis',(0.,-1.,0.));
#5670=DIRECTION('ref_axis',(0.707106781186547,0.,0.707106781186548));
#5671=DIRECTION('center_axis',(1.,0.,0.));
#5672=DIRECTION('ref_axis',(0.,-1.,1.22464679914735E-16));
#5673=DIRECTION('center_axis',(0.,-0.043896042544273,-0.999036104176897));
#5674=DIRECTION('ref_axis',(-1.,0.,0.));
#5675=DIRECTION('center_axis',(0.,-0.0438960425442462,0.999036104176898));
#5676=DIRECTION('ref_axis',(-0.321450532286738,0.946013634312855,0.0415663203417933));
#5677=DIRECTION('center_axis',(0.,1.,0.));
#5678=DIRECTION('ref_axis',(-0.707106781186548,0.,0.707106781186547));
#5679=DIRECTION('',(0.,1.,0.));
#5680=DIRECTION('center_axis',(0.,-1.,0.));
#5681=DIRECTION('ref_axis',(4.7642445544227E-13,0.,1.));
#5682=DIRECTION('center_axis',(-0.413050977203529,0.295699193086847,-0.861365704819386));
#5683=DIRECTION('ref_axis',(-0.700390161752567,0.501402531664142,0.507985356640329));
#5684=DIRECTION('center_axis',(-0.946831936616679,-0.321728587170473,0.));
#5685=DIRECTION('ref_axis',(-3.02535774210343E-14,-1.77635683940018E-14,
1.));
#5686=DIRECTION('center_axis',(0.413050977203297,-0.295699193086435,-0.861365704819639));
#5687=DIRECTION('ref_axis',(-0.700390161752968,0.501402531664014,-0.507985356639902));
#5688=DIRECTION('center_axis',(-0.946831936616687,-0.321728587170451,0.));
#5689=DIRECTION('ref_axis',(1.69586567011493E-13,8.88178419700125E-14,-1.));
#5690=DIRECTION('center_axis',(0.,0.,-1.));
#5691=DIRECTION('ref_axis',(-1.,0.,0.));
#5692=DIRECTION('',(0.,-1.,0.));
#5693=DIRECTION('center_axis',(1.,0.,0.));
#5694=DIRECTION('ref_axis',(0.,1.,0.));
#5695=DIRECTION('center_axis',(-1.,0.,0.));
#5696=DIRECTION('ref_axis',(0.,0.,1.));
#5697=DIRECTION('center_axis',(-1.,0.,0.));
#5698=DIRECTION('ref_axis',(0.,-1.,1.22464679914735E-16));
#5699=DIRECTION('axis',(0.,0.,1.));
#5700=DIRECTION('refdir',(1.,0.,0.));
#5701=DIRECTION('center_axis',(1.,0.,0.));
#5702=DIRECTION('ref_axis',(0.,-1.,0.));
#5703=DIRECTION('center_axis',(-1.,0.,0.));
#5704=DIRECTION('ref_axis',(0.,-1.,0.));
#5705=DIRECTION('center_axis',(-1.,0.,0.));
#5706=DIRECTION('ref_axis',(0.,-1.,0.));
#5707=DIRECTION('',(-0.70710678118655,-0.707106781186545,-8.6595605623549E-17));
#5708=DIRECTION('center_axis',(1.,0.,0.));
#5709=DIRECTION('ref_axis',(0.,-1.,0.));
#5710=DIRECTION('center_axis',(1.,0.,0.));
#5711=DIRECTION('ref_axis',(0.,1.,0.));
#5712=DIRECTION('center_axis',(1.,0.,0.));
#5713=DIRECTION('ref_axis',(0.,-1.,0.));
#5714=DIRECTION('center_axis',(1.,0.,0.));
#5715=DIRECTION('ref_axis',(0.,-1.,0.));
#5716=DIRECTION('',(-1.,0.,0.));
#5717=DIRECTION('center_axis',(-1.,0.,0.));
#5718=DIRECTION('ref_axis',(0.,0.,1.));
#5719=DIRECTION('center_axis',(1.,0.,0.));
#5720=DIRECTION('ref_axis',(0.,0.,-1.));
#5721=DIRECTION('center_axis',(-1.,0.,0.));
#5722=DIRECTION('ref_axis',(0.,-1.,0.));
#5723=DIRECTION('center_axis',(-1.,0.,0.));
#5724=DIRECTION('ref_axis',(0.,-1.,0.));
#5725=DIRECTION('',(-0.70710678118655,0.707106781186545,8.6595605623549E-17));
#5726=DIRECTION('center_axis',(1.,0.,0.));
#5727=DIRECTION('ref_axis',(0.,0.,-1.));
#5728=DIRECTION('center_axis',(-1.,0.,0.));
#5729=DIRECTION('ref_axis',(0.,-1.,1.83697019872103E-16));
#5730=DIRECTION('center_axis',(1.,0.,0.));
#5731=DIRECTION('ref_axis',(0.,1.,0.));
#5732=DIRECTION('',(1.,0.,0.));
#5733=DIRECTION('center_axis',(1.,0.,0.));
#5734=DIRECTION('ref_axis',(0.,0.,-1.));
#5735=DIRECTION('',(-1.,0.,0.));
#5736=DIRECTION('center_axis',(1.,0.,0.));
#5737=DIRECTION('ref_axis',(0.,0.,-1.));
#5738=DIRECTION('center_axis',(1.,0.,0.));
#5739=DIRECTION('ref_axis',(0.,1.,0.));
#5740=DIRECTION('',(-1.,0.,0.));
#5741=DIRECTION('center_axis',(1.,0.,0.));
#5742=DIRECTION('ref_axis',(0.,0.,-1.));
#5743=DIRECTION('',(1.,0.,0.));
#5744=DIRECTION('center_axis',(1.,0.,0.));
#5745=DIRECTION('ref_axis',(0.,0.,-1.));
#5746=DIRECTION('center_axis',(1.,0.,0.));
#5747=DIRECTION('ref_axis',(0.,0.,-1.));
#5748=DIRECTION('',(0.,0.,-1.));
#5749=DIRECTION('',(0.,-1.,0.));
#5750=DIRECTION('center_axis',(1.,0.,0.));
#5751=DIRECTION('ref_axis',(0.,0.,-1.));
#5752=DIRECTION('',(0.,0.,-1.));
#5753=DIRECTION('',(0.,1.,0.));
#5754=DIRECTION('center_axis',(-1.,0.,0.));
#5755=DIRECTION('ref_axis',(0.,0.,1.));
#5756=DIRECTION('',(0.,0.,1.));
#5757=DIRECTION('',(0.,1.,0.));
#5758=DIRECTION('center_axis',(-1.,0.,0.));
#5759=DIRECTION('ref_axis',(0.,0.,1.));
#5760=DIRECTION('',(0.,0.,1.));
#5761=DIRECTION('',(0.,-1.,0.));
#5762=DIRECTION('center_axis',(0.,0.,1.));
#5763=DIRECTION('ref_axis',(1.,0.,0.));
#5764=DIRECTION('',(-1.,0.,0.));
#5765=DIRECTION('',(0.,1.,0.));
#5766=DIRECTION('',(1.,0.,0.));
#5767=DIRECTION('',(0.,-1.,0.));
#5768=DIRECTION('',(1.,0.,0.));
#5769=DIRECTION('',(-1.,0.,0.));
#5770=DIRECTION('center_axis',(1.,0.,0.));
#5771=DIRECTION('ref_axis',(0.,0.,-1.));
#5772=DIRECTION('center_axis',(-1.,0.,0.));
#5773=DIRECTION('ref_axis',(0.,-1.,3.06161699786838E-17));
#5774=DIRECTION('center_axis',(-1.,0.,0.));
#5775=DIRECTION('ref_axis',(0.,-1.,3.06161699786838E-17));
#5776=DIRECTION('center_axis',(0.,-1.,-1.22464679914735E-16));
#5777=DIRECTION('ref_axis',(0.,-1.22464679914735E-16,1.));
#5778=DIRECTION('center_axis',(1.,0.,0.));
#5779=DIRECTION('ref_axis',(0.,-1.,1.83697019872103E-16));
#5780=DIRECTION('center_axis',(1.,0.,0.));
#5781=DIRECTION('ref_axis',(0.,-1.,1.83697019872103E-16));
#5782=DIRECTION('center_axis',(1.,0.,0.));
#5783=DIRECTION('ref_axis',(0.,1.,0.));
#5784=DIRECTION('',(-1.,0.,0.));
#5785=DIRECTION('center_axis',(-1.,0.,0.));
#5786=DIRECTION('ref_axis',(0.,1.,0.));
#5787=DIRECTION('center_axis',(1.,0.,0.));
#5788=DIRECTION('ref_axis',(0.,-1.,3.06161699786838E-17));
#5789=DIRECTION('',(-0.707106781186546,-0.707106781186549,-8.65956056235495E-17));
#5790=DIRECTION('center_axis',(1.,0.,0.));
#5791=DIRECTION('ref_axis',(0.,-1.,3.06161699786838E-17));
#5792=DIRECTION('center_axis',(1.,0.,0.));
#5793=DIRECTION('ref_axis',(0.,0.,-1.));
#5794=DIRECTION('center_axis',(0.,-1.,-1.22464679914735E-16));
#5795=DIRECTION('ref_axis',(0.,-1.22464679914735E-16,1.));
#5796=DIRECTION('center_axis',(1.,0.,0.));
#5797=DIRECTION('ref_axis',(0.,-1.,1.83697019872103E-16));
#5798=DIRECTION('center_axis',(1.,0.,0.));
#5799=DIRECTION('ref_axis',(0.,-1.,1.83697019872103E-16));
#5800=DIRECTION('center_axis',(1.,0.,0.));
#5801=DIRECTION('ref_axis',(0.,1.,0.));
#5802=DIRECTION('',(-1.,0.,0.));
#5803=DIRECTION('center_axis',(-1.,0.,0.));
#5804=DIRECTION('ref_axis',(0.,-1.,1.83697019872103E-16));
#5805=DIRECTION('',(-1.,0.,0.));
#5806=DIRECTION('center_axis',(-1.,0.,0.));
#5807=DIRECTION('ref_axis',(0.,-1.,1.83697019872103E-16));
#5808=DIRECTION('center_axis',(1.,0.,0.));
#5809=DIRECTION('ref_axis',(0.,-1.,-6.12323399573677E-17));
#5810=DIRECTION('center_axis',(1.,0.,0.));
#5811=DIRECTION('ref_axis',(0.,-1.,3.06161699786838E-17));
#5812=DIRECTION('center_axis',(1.,0.,0.));
#5813=DIRECTION('ref_axis',(0.,-1.,1.22464679914735E-16));
#5814=DIRECTION('center_axis',(-1.,0.,0.));
#5815=DIRECTION('ref_axis',(0.,-1.,3.06161699786838E-17));
#5816=DIRECTION('center_axis',(0.692464013941372,0.721452416584908,-7.14974227561921E-12));
#5817=DIRECTION('ref_axis',(-1.03250741290139E-11,0.,-1.));
#5818=DIRECTION('center_axis',(0.692464013941369,0.721452416584911,7.14974227561918E-12));
#5819=DIRECTION('ref_axis',(-0.70710678118655,0.678694795014786,-0.198427254226414));
#5820=DIRECTION('center_axis',(1.,0.,0.));
#5821=DIRECTION('ref_axis',(0.,-1.,-1.17055854380544E-13));
#5822=DIRECTION('center_axis',(3.44290678714761E-15,-0.280618514071671,
0.959819383821877));
#5823=DIRECTION('ref_axis',(-0.707106781186548,0.678694795014742,0.198427254226573));
#5824=DIRECTION('center_axis',(1.,0.,0.));
#5825=DIRECTION('ref_axis',(0.,-1.,1.83697019872103E-16));
#5826=DIRECTION('center_axis',(6.88581357429522E-15,-0.28061851407167,-0.959819383821877));
#5827=DIRECTION('ref_axis',(-1.,-5.55111512312578E-15,-5.55111512312578E-15));
#5828=DIRECTION('center_axis',(-0.371626520792815,0.147747632515864,-0.91655025292091));
#5829=DIRECTION('ref_axis',(-0.851707287237021,0.338613441842967,0.399919534244846));
#5830=DIRECTION('center_axis',(0.,1.,0.));
#5831=DIRECTION('ref_axis',(-0.707106781186545,0.,0.70710678118655));
#5832=DIRECTION('center_axis',(0.371626520793064,-0.147747632509487,-0.916550252921837));
#5833=DIRECTION('ref_axis',(-0.851707287242982,0.338613441830485,-0.39991953424272));
#5834=DIRECTION('center_axis',(0.,1.,0.));
#5835=DIRECTION('ref_axis',(-0.707106781186545,0.,-0.70710678118655));
#5836=DIRECTION('center_axis',(0.,0.,-1.));
#5837=DIRECTION('ref_axis',(-1.,0.,0.));
#5838=DIRECTION('',(1.,0.,0.));
#5839=DIRECTION('',(0.,1.,0.));
#5840=DIRECTION('',(-1.,0.,0.));
#5841=DIRECTION('',(0.,-1.,0.));
#5842=DIRECTION('',(1.,0.,0.));
#5843=DIRECTION('center_axis',(0.,1.,0.));
#5844=DIRECTION('ref_axis',(-0.70710678118654,0.,0.707106781186555));
#5845=DIRECTION('',(0.,-1.,0.));
#5846=DIRECTION('center_axis',(0.,-1.,0.));
#5847=DIRECTION('ref_axis',(-1.,0.,0.));
#5848=DIRECTION('center_axis',(-1.,0.,0.));
#5849=DIRECTION('ref_axis',(0.,0.,1.));
#5850=DIRECTION('',(0.,1.,0.));
#5851=DIRECTION('center_axis',(-1.,0.,0.));
#5852=DIRECTION('ref_axis',(0.,-1.,1.83697019872103E-16));
#5853=DIRECTION('center_axis',(0.,-1.,0.));
#5854=DIRECTION('ref_axis',(-0.70710678118654,0.,-0.707106781186555));
#5855=DIRECTION('center_axis',(0.,-1.,0.));
#5856=DIRECTION('ref_axis',(0.,0.,-1.));
#5857=DIRECTION('center_axis',(1.,0.,0.));
#5858=DIRECTION('ref_axis',(0.,0.,-1.));
#5859=DIRECTION('center_axis',(-1.,0.,0.));
#5860=DIRECTION('ref_axis',(0.,-1.,1.83697019872103E-16));
#5861=DIRECTION('center_axis',(0.,-1.,-1.22464679914735E-16));
#5862=DIRECTION('ref_axis',(0.,-1.22464679914735E-16,1.));
#5863=DIRECTION('center_axis',(1.,0.,0.));
#5864=DIRECTION('ref_axis',(0.,0.,-1.));
#5865=DIRECTION('center_axis',(1.,0.,0.));
#5866=DIRECTION('ref_axis',(0.,-1.,1.83697019872103E-16));
#5867=DIRECTION('center_axis',(1.,0.,0.));
#5868=DIRECTION('ref_axis',(0.,0.,-1.));
#5869=DIRECTION('center_axis',(-1.,0.,0.));
#5870=DIRECTION('ref_axis',(0.,-1.,1.83697019872103E-16));
#5871=DIRECTION('center_axis',(-1.,0.,0.));
#5872=DIRECTION('ref_axis',(0.,-1.,1.83697019872103E-16));
#5873=DIRECTION('center_axis',(0.,-1.,-1.22464679914735E-16));
#5874=DIRECTION('ref_axis',(0.,-1.22464679914735E-16,1.));
#5875=DIRECTION('center_axis',(1.,0.,0.));
#5876=DIRECTION('ref_axis',(0.,1.,0.));
#5877=DIRECTION('',(-1.,0.,0.));
#5878=DIRECTION('center_axis',(1.,0.,0.));
#5879=DIRECTION('ref_axis',(0.,-1.,1.83697019872103E-16));
#5880=DIRECTION('',(-1.,0.,0.));
#5881=DIRECTION('center_axis',(1.,0.,0.));
#5882=DIRECTION('ref_axis',(0.,1.,0.));
#5883=DIRECTION('',(1.,0.,0.));
#5884=DIRECTION('center_axis',(1.,0.,0.));
#5885=DIRECTION('ref_axis',(0.,-1.,1.83697019872103E-16));
#5886=DIRECTION('center_axis',(0.,1.,0.));
#5887=DIRECTION('ref_axis',(-1.,0.,0.));
#5888=DIRECTION('',(0.,0.,1.));
#5889=DIRECTION('center_axis',(0.290768000350851,-0.8729165634249,-0.391753293885871));
#5890=DIRECTION('ref_axis',(-0.520254270210838,-0.48786952487162,0.700941382020586));
#5891=DIRECTION('center_axis',(-1.,0.,0.));
#5892=DIRECTION('ref_axis',(0.,0.,1.));
#5893=DIRECTION('center_axis',(0.,0.347305389221559,0.937752081638672));
#5894=DIRECTION('ref_axis',(0.,-0.937752081638672,0.347305389221559));
#5895=DIRECTION('center_axis',(0.290768000350852,-0.872916563424899,0.391753293885873));
#5896=DIRECTION('ref_axis',(-0.520254270210838,-0.487869524871625,-0.700941382020582));
#5897=DIRECTION('center_axis',(-1.,0.,0.));
#5898=DIRECTION('ref_axis',(0.,-0.937752081638672,-0.347305389221556));
#5899=DIRECTION('center_axis',(0.,0.347305389221548,-0.937752081638676));
#5900=DIRECTION('ref_axis',(-1.,0.,0.));
#5901=DIRECTION('center_axis',(1.,0.,0.));
#5902=DIRECTION('ref_axis',(0.,-1.,-6.12323399573677E-17));
#5903=DIRECTION('center_axis',(-1.,0.,0.));
#5904=DIRECTION('ref_axis',(0.,-0.57126815541322,0.820763482746874));
#5905=DIRECTION('center_axis',(-1.,0.,0.));
#5906=DIRECTION('ref_axis',(0.,0.,1.));
#5907=DIRECTION('center_axis',(-1.,0.,0.));
#5908=DIRECTION('ref_axis',(0.,1.,0.));
#5909=DIRECTION('center_axis',(1.,0.,0.));
#5910=DIRECTION('ref_axis',(0.,-0.57126815541322,-0.820763482746874));
#5911=DIRECTION('center_axis',(1.,0.,0.));
#5912=DIRECTION('ref_axis',(0.,1.,0.));
#5913=DIRECTION('axis',(0.,0.,1.));
#5914=DIRECTION('refdir',(1.,0.,0.));
#5915=DIRECTION('center_axis',(1.,0.,0.));
#5916=DIRECTION('ref_axis',(0.,0.,-1.));
#5917=DIRECTION('center_axis',(-1.,0.,0.));
#5918=DIRECTION('ref_axis',(0.,-1.,1.83697019872103E-16));
#5919=DIRECTION('center_axis',(0.,-1.,-1.22464679914735E-16));
#5920=DIRECTION('ref_axis',(0.,-1.22464679914735E-16,1.));
#5921=DIRECTION('center_axis',(1.,0.,0.));
#5922=DIRECTION('ref_axis',(0.,-1.,3.06161699786838E-17));
#5923=DIRECTION('center_axis',(1.,0.,0.));
#5924=DIRECTION('ref_axis',(0.,-1.,3.06161699786838E-17));
#5925=DIRECTION('center_axis',(-1.,0.,0.));
#5926=DIRECTION('ref_axis',(0.,1.,0.));
#5927=DIRECTION('',(-0.707106781186546,-0.707106781186549,-8.65956056235495E-17));
#5928=DIRECTION('center_axis',(-1.,0.,0.));
#5929=DIRECTION('ref_axis',(0.,-1.,3.06161699786838E-17));
#5930=DIRECTION('center_axis',(-1.,0.,0.));
#5931=DIRECTION('ref_axis',(0.,-1.,3.06161699786838E-17));
#5932=DIRECTION('center_axis',(1.,0.,0.));
#5933=DIRECTION('ref_axis',(0.,0.,-1.));
#5934=DIRECTION('center_axis',(1.,0.,0.));
#5935=DIRECTION('ref_axis',(0.,-1.,1.83697019872103E-16));
#5936=DIRECTION('center_axis',(1.,0.,0.));
#5937=DIRECTION('ref_axis',(0.,0.,-1.));
#5938=DIRECTION('center_axis',(0.,-1.,-1.22464679914735E-16));
#5939=DIRECTION('ref_axis',(0.,-1.22464679914735E-16,1.));
#5940=DIRECTION('center_axis',(1.,0.,0.));
#5941=DIRECTION('ref_axis',(0.,-1.,1.83697019872103E-16));
#5942=DIRECTION('center_axis',(1.,0.,0.));
#5943=DIRECTION('ref_axis',(0.,-1.,1.83697019872103E-16));
#5944=DIRECTION('center_axis',(1.,0.,0.));
#5945=DIRECTION('ref_axis',(0.,1.,0.));
#5946=DIRECTION('',(-1.,0.,0.));
#5947=DIRECTION('center_axis',(-1.,0.,0.));
#5948=DIRECTION('ref_axis',(0.,-1.,1.83697019872103E-16));
#5949=DIRECTION('center_axis',(-1.,0.,0.));
#5950=DIRECTION('ref_axis',(0.,-1.,1.83697019872103E-16));
#5951=DIRECTION('center_axis',(1.,0.,0.));
#5952=DIRECTION('ref_axis',(0.,0.,-1.));
#5953=DIRECTION('center_axis',(0.,-1.,-1.22464679914735E-16));
#5954=DIRECTION('ref_axis',(0.,-1.22464679914735E-16,1.));
#5955=DIRECTION('center_axis',(1.,0.,0.));
#5956=DIRECTION('ref_axis',(0.,-1.,1.83697019872103E-16));
#5957=DIRECTION('center_axis',(-1.,0.,0.));
#5958=DIRECTION('ref_axis',(0.,0.,1.));
#5959=DIRECTION('center_axis',(-1.,0.,0.));
#5960=DIRECTION('ref_axis',(0.,-1.,1.83697019872103E-16));
#5961=DIRECTION('center_axis',(1.,0.,0.));
#5962=DIRECTION('ref_axis',(0.,0.,-1.));
#5963=DIRECTION('center_axis',(0.,-1.,-1.22464679914735E-16));
#5964=DIRECTION('ref_axis',(0.,-1.22464679914735E-16,1.));
#5965=DIRECTION('center_axis',(1.,0.,0.));
#5966=DIRECTION('ref_axis',(0.,-1.,1.83697019872103E-16));
#5967=DIRECTION('center_axis',(1.,0.,0.));
#5968=DIRECTION('ref_axis',(0.,-1.,1.83697019872103E-16));
#5969=DIRECTION('center_axis',(1.,0.,0.));
#5970=DIRECTION('ref_axis',(0.,1.,0.));
#5971=DIRECTION('center_axis',(-1.,0.,0.));
#5972=DIRECTION('ref_axis',(0.,-1.,1.83697019872103E-16));
#5973=DIRECTION('center_axis',(-1.,0.,0.));
#5974=DIRECTION('ref_axis',(0.,-1.,1.83697019872103E-16));
#5975=DIRECTION('',(-1.,0.,0.));
#5976=DIRECTION('center_axis',(1.,0.,0.));
#5977=DIRECTION('ref_axis',(0.,0.,-1.));
#5978=DIRECTION('center_axis',(0.,-1.,-1.22464679914735E-16));
#5979=DIRECTION('ref_axis',(0.,-1.22464679914735E-16,1.));
#5980=DIRECTION('axis',(0.,0.,1.));
#5981=DIRECTION('refdir',(1.,0.,0.));
#5982=DIRECTION('center_axis',(1.,0.,0.));
#5983=DIRECTION('ref_axis',(0.,1.,0.));
#5984=DIRECTION('center_axis',(1.,0.,0.));
#5985=DIRECTION('ref_axis',(0.,0.,-1.));
#5986=DIRECTION('',(-1.,0.,0.));
#5987=DIRECTION('center_axis',(1.,0.,0.));
#5988=DIRECTION('ref_axis',(0.,0.,-1.));
#5989=DIRECTION('center_axis',(1.,0.,0.));
#5990=DIRECTION('ref_axis',(0.,0.,-1.));
#5991=DIRECTION('center_axis',(1.,0.,0.));
#5992=DIRECTION('ref_axis',(0.,0.,-1.));
#5993=DIRECTION('center_axis',(1.,0.,0.));
#5994=DIRECTION('ref_axis',(0.,1.,0.));
#5995=DIRECTION('',(-0.70710678118655,0.707106781186545,8.6595605623549E-17));
#5996=DIRECTION('center_axis',(1.,0.,0.));
#5997=DIRECTION('ref_axis',(0.,0.,-1.));
#5998=DIRECTION('center_axis',(1.,0.,0.));
#5999=DIRECTION('ref_axis',(0.,1.,0.));
#6000=DIRECTION('',(-1.,0.,0.));
#6001=DIRECTION('center_axis',(1.,0.,0.));
#6002=DIRECTION('ref_axis',(0.,0.,-1.));
#6003=DIRECTION('center_axis',(-1.,0.,0.));
#6004=DIRECTION('ref_axis',(0.,1.,0.));
#6005=DIRECTION('',(-0.707106781186548,-0.707106781186548,-8.65956056235493E-17));
#6006=DIRECTION('center_axis',(1.,0.,0.));
#6007=DIRECTION('ref_axis',(0.,0.,-1.));
#6008=DIRECTION('center_axis',(-1.,0.,0.));
#6009=DIRECTION('ref_axis',(0.,0.,1.));
#6010=DIRECTION('axis',(0.,0.,1.));
#6011=DIRECTION('refdir',(1.,0.,0.));
#6012=DIRECTION('center_axis',(1.,0.,0.));
#6013=DIRECTION('ref_axis',(0.,1.,0.));
#6014=DIRECTION('center_axis',(1.,0.,0.));
#6015=DIRECTION('ref_axis',(0.,0.,-1.));
#6016=DIRECTION('',(-0.707106781186547,0.707106781186548,8.65956056235494E-17));
#6017=DIRECTION('center_axis',(1.,0.,0.));
#6018=DIRECTION('ref_axis',(0.,0.,-1.));
#6019=DIRECTION('center_axis',(1.,0.,0.));
#6020=DIRECTION('ref_axis',(0.,1.,0.));
#6021=DIRECTION('center_axis',(1.,0.,0.));
#6022=DIRECTION('ref_axis',(0.,0.,-1.));
#6023=DIRECTION('',(-1.,0.,0.));
#6024=DIRECTION('center_axis',(-1.,0.,0.));
#6025=DIRECTION('ref_axis',(0.,1.,0.));
#6026=DIRECTION('center_axis',(1.,0.,0.));
#6027=DIRECTION('ref_axis',(0.,0.,-1.));
#6028=DIRECTION('',(-0.707106781186547,-0.707106781186547,-8.65956056235493E-17));
#6029=DIRECTION('center_axis',(1.,0.,0.));
#6030=DIRECTION('ref_axis',(0.,0.,-1.));
#6031=DIRECTION('center_axis',(1.,0.,0.));
#6032=DIRECTION('ref_axis',(0.,0.,-1.));
#6033=DIRECTION('center_axis',(1.,0.,0.));
#6034=DIRECTION('ref_axis',(0.,1.,0.));
#6035=DIRECTION('',(-1.,0.,0.));
#6036=DIRECTION('center_axis',(1.,0.,0.));
#6037=DIRECTION('ref_axis',(0.,0.,-1.));
#6038=DIRECTION('center_axis',(-1.,0.,0.));
#6039=DIRECTION('ref_axis',(0.,0.,1.));
#6040=DIRECTION('axis',(0.,0.,1.));
#6041=DIRECTION('refdir',(1.,0.,0.));
#6042=DIRECTION('center_axis',(1.,0.,0.));
#6043=DIRECTION('ref_axis',(0.,0.,-1.));
#6044=DIRECTION('center_axis',(1.,0.,0.));
#6045=DIRECTION('ref_axis',(0.,0.,-1.));
#6046=DIRECTION('',(1.,0.,0.));
#6047=DIRECTION('center_axis',(-1.,0.,0.));
#6048=DIRECTION('ref_axis',(0.,0.,-1.));
#6049=DIRECTION('center_axis',(1.,0.,0.));
#6050=DIRECTION('ref_axis',(0.,0.,-1.));
#6051=DIRECTION('center_axis',(1.,0.,0.));
#6052=DIRECTION('ref_axis',(0.,0.,-1.));
#6053=DIRECTION('',(1.,0.,0.));
#6054=DIRECTION('center_axis',(-1.,0.,0.));
#6055=DIRECTION('ref_axis',(0.,0.,-1.));
#6056=DIRECTION('center_axis',(1.,0.,0.));
#6057=DIRECTION('ref_axis',(0.,0.,-1.));
#6058=DIRECTION('',(0.,1.,0.));
#6059=DIRECTION('',(0.,0.,1.));
#6060=DIRECTION('',(0.,-1.,0.));
#6061=DIRECTION('center_axis',(1.,0.,0.));
#6062=DIRECTION('ref_axis',(0.,0.,-1.));
#6063=DIRECTION('',(0.,1.,0.));
#6064=DIRECTION('',(0.,0.,1.));
#6065=DIRECTION('',(0.,-1.,0.));
#6066=DIRECTION('center_axis',(1.,0.,0.));
#6067=DIRECTION('ref_axis',(0.,0.,-1.));
#6068=DIRECTION('center_axis',(0.,0.,1.));
#6069=DIRECTION('ref_axis',(0.,-1.,0.));
#6070=DIRECTION('',(1.,0.,0.));
#6071=DIRECTION('',(0.,1.,0.));
#6072=DIRECTION('',(-1.,0.,0.));
#6073=DIRECTION('center_axis',(0.,1.,0.));
#6074=DIRECTION('ref_axis',(0.,0.,1.));
#6075=DIRECTION('',(0.,0.,-1.));
#6076=DIRECTION('',(1.,0.,0.));
#6077=DIRECTION('center_axis',(0.,0.,-1.));
#6078=DIRECTION('ref_axis',(0.,1.,0.));
#6079=DIRECTION('',(1.,0.,0.));
#6080=DIRECTION('',(0.,-1.,0.));
#6081=DIRECTION('center_axis',(-1.,0.,0.));
#6082=DIRECTION('ref_axis',(0.,0.,1.));
#6083=DIRECTION('',(0.,-1.,0.));
#6084=DIRECTION('center_axis',(1.,0.,0.));
#6085=DIRECTION('ref_axis',(0.,0.,-1.));
#6086=DIRECTION('center_axis',(1.,0.,0.));
#6087=DIRECTION('ref_axis',(0.,0.,-1.));
#6088=DIRECTION('',(0.,-1.,0.));
#6089=DIRECTION('',(0.,0.,1.));
#6090=DIRECTION('center_axis',(1.,0.,0.));
#6091=DIRECTION('ref_axis',(0.,-1.,-1.22464679914735E-16));
#6092=DIRECTION('',(-1.,0.,0.));
#6093=DIRECTION('center_axis',(0.,0.,1.));
#6094=DIRECTION('ref_axis',(0.,-1.,0.));
#6095=DIRECTION('',(1.,0.,0.));
#6096=DIRECTION('center_axis',(0.,0.,-1.));
#6097=DIRECTION('ref_axis',(0.,1.,0.));
#6098=DIRECTION('',(1.,0.,0.));
#6099=DIRECTION('',(1.,0.,0.));
#6100=DIRECTION('center_axis',(0.,1.,0.));
#6101=DIRECTION('ref_axis',(0.,0.,1.));
#6102=DIRECTION('center_axis',(1.,0.,0.));
#6103=DIRECTION('ref_axis',(0.,-1.,1.22464679914735E-16));
#6104=DIRECTION('axis',(0.,0.,1.));
#6105=DIRECTION('refdir',(1.,0.,0.));
#6106=DIRECTION('center_axis',(0.577350269189626,0.577350269189624,0.577350269189627));
#6107=DIRECTION('ref_axis',(0.707106781186548,0.,-0.707106781186547));
#6108=DIRECTION('',(-0.707106781186548,0.,0.707106781186547));
#6109=DIRECTION('',(0.707106781186546,-0.707106781186549,0.));
#6110=DIRECTION('',(3.14018491736755E-15,0.707106781186548,-0.707106781186547));
#6111=DIRECTION('center_axis',(0.577350269189625,-0.577350269189626,0.577350269189626));
#6112=DIRECTION('ref_axis',(0.707106781186548,0.,-0.707106781186547));
#6113=DIRECTION('',(0.,0.707106781186547,0.707106781186548));
#6114=DIRECTION('',(-0.707106781186548,-0.707106781186547,0.));
#6115=DIRECTION('',(0.707106781186548,0.,-0.707106781186547));
#6116=DIRECTION('center_axis',(-0.577350269189626,0.577350269189626,0.577350269189626));
#6117=DIRECTION('ref_axis',(0.707106781186547,0.,0.707106781186547));
#6118=DIRECTION('',(0.,-0.707106781186548,0.707106781186547));
#6119=DIRECTION('',(0.707106781186547,0.707106781186547,0.));
#6120=DIRECTION('',(-0.707106781186547,0.,-0.707106781186547));
#6121=DIRECTION('center_axis',(0.577350269189626,0.577350269189624,-0.577350269189627));
#6122=DIRECTION('ref_axis',(-0.707106781186548,0.,-0.707106781186547));
#6123=DIRECTION('',(-3.14018491736755E-15,-0.707106781186548,-0.707106781186547));
#6124=DIRECTION('',(-0.707106781186546,0.707106781186549,0.));
#6125=DIRECTION('',(0.707106781186548,0.,0.707106781186547));
#6126=DIRECTION('center_axis',(0.707106781186549,0.707106781186546,0.));
#6127=DIRECTION('ref_axis',(0.,0.,-1.));
#6128=DIRECTION('',(0.,0.,-1.));
#6129=DIRECTION('',(0.,0.,1.));
#6130=DIRECTION('center_axis',(-0.577350269189627,-0.577350269189625,0.577350269189625));
#6131=DIRECTION('ref_axis',(0.707106781186546,0.,0.707106781186549));
#6132=DIRECTION('',(0.707106781186547,-3.14018491736755E-15,0.707106781186547));
#6133=DIRECTION('',(-0.707106781186546,0.707106781186549,0.));
#6134=DIRECTION('',(0.,-0.707106781186547,-0.707106781186548));
#6135=DIRECTION('center_axis',(0.577350269189625,-0.577350269189627,-0.577350269189626));
#6136=DIRECTION('ref_axis',(-0.707106781186548,0.,-0.707106781186547));
#6137=DIRECTION('',(-0.707106781186548,0.,-0.707106781186547));
#6138=DIRECTION('',(0.707106781186548,0.707106781186547,0.));
#6139=DIRECTION('',(0.,-0.707106781186547,0.707106781186548));
#6140=DIRECTION('center_axis',(0.707106781186547,-0.707106781186548,0.));
#6141=DIRECTION('ref_axis',(0.,0.,-1.));
#6142=DIRECTION('',(0.,0.,-1.));
#6143=DIRECTION('',(0.,0.,1.));
#6144=DIRECTION('center_axis',(-0.577350269189626,0.577350269189626,-0.577350269189626));
#6145=DIRECTION('ref_axis',(-0.707106781186548,0.,0.707106781186547));
#6146=DIRECTION('',(0.707106781186547,0.,-0.707106781186547));
#6147=DIRECTION('',(-0.707106781186547,-0.707106781186547,0.));
#6148=DIRECTION('',(0.,0.707106781186548,0.707106781186547));
#6149=DIRECTION('center_axis',(-0.707106781186548,0.707106781186548,0.));
#6150=DIRECTION('ref_axis',(0.,0.,1.));
#6151=DIRECTION('',(0.,0.,1.));
#6152=DIRECTION('',(0.,0.,-1.));
#6153=DIRECTION('center_axis',(0.,0.707106781186547,-0.707106781186548));
#6154=DIRECTION('ref_axis',(-1.,0.,0.));
#6155=DIRECTION('',(-1.,0.,0.));
#6156=DIRECTION('',(1.,0.,0.));
#6157=DIRECTION('center_axis',(-0.577350269189627,-0.577350269189625,-0.577350269189625));
#6158=DIRECTION('ref_axis',(-0.707106781186546,0.,0.707106781186549));
#6159=DIRECTION('',(0.,0.707106781186547,-0.707106781186548));
#6160=DIRECTION('',(0.707106781186546,-0.707106781186549,0.));
#6161=DIRECTION('',(-0.707106781186547,3.14018491736755E-15,0.707106781186547));
#6162=DIRECTION('center_axis',(-0.707106781186549,-0.707106781186546,0.));
#6163=DIRECTION('ref_axis',(0.,0.,1.));
#6164=DIRECTION('',(0.,0.,-1.));
#6165=DIRECTION('',(0.,0.,1.));
#6166=DIRECTION('center_axis',(-0.707106781186548,0.,-0.707106781186548));
#6167=DIRECTION('ref_axis',(-0.707106781186548,0.,0.707106781186548));
#6168=DIRECTION('',(0.,-1.,0.));
#6169=DIRECTION('',(0.,1.,0.));
#6170=DIRECTION('center_axis',(0.,-0.707106781186548,-0.707106781186547));
#6171=DIRECTION('ref_axis',(-1.,0.,0.));
#6172=DIRECTION('',(1.,0.,0.));
#6173=DIRECTION('',(-1.,0.,0.));
#6174=DIRECTION('center_axis',(0.707106781186547,0.,-0.707106781186548));
#6175=DIRECTION('ref_axis',(-0.707106781186548,0.,-0.707106781186547));
#6176=DIRECTION('',(0.,1.,0.));
#6177=DIRECTION('',(0.,-1.,0.));
#6178=DIRECTION('center_axis',(0.,-0.707106781186548,0.707106781186547));
#6179=DIRECTION('ref_axis',(1.,0.,0.));
#6180=DIRECTION('',(-1.,0.,0.));
#6181=DIRECTION('',(1.,0.,0.));
#6182=DIRECTION('center_axis',(-0.707106781186548,0.,0.707106781186548));
#6183=DIRECTION('ref_axis',(0.707106781186548,0.,0.707106781186548));
#6184=DIRECTION('',(0.,1.,0.));
#6185=DIRECTION('',(0.,-1.,0.));
#6186=DIRECTION('center_axis',(0.,0.707106781186547,0.707106781186548));
#6187=DIRECTION('ref_axis',(1.,0.,0.));
#6188=DIRECTION('',(1.,0.,0.));
#6189=DIRECTION('',(-1.,0.,0.));
#6190=DIRECTION('center_axis',(0.707106781186547,0.,0.707106781186548));
#6191=DIRECTION('ref_axis',(0.707106781186548,0.,-0.707106781186547));
#6192=DIRECTION('',(0.,-1.,0.));
#6193=DIRECTION('',(0.,1.,0.));
#6194=DIRECTION('center_axis',(1.,0.,0.));
#6195=DIRECTION('ref_axis',(0.,1.,0.));
#6196=DIRECTION('center_axis',(0.,1.,0.));
#6197=DIRECTION('ref_axis',(-1.,0.,0.));
#6198=DIRECTION('center_axis',(0.,0.,-1.));
#6199=DIRECTION('ref_axis',(-1.,0.,0.));
#6200=DIRECTION('center_axis',(0.,-1.,0.));
#6201=DIRECTION('ref_axis',(1.,0.,0.));
#6202=DIRECTION('center_axis',(-1.,0.,0.));
#6203=DIRECTION('ref_axis',(0.,-1.,0.));
#6204=DIRECTION('center_axis',(0.,0.,1.));
#6205=DIRECTION('ref_axis',(1.,0.,0.));
#6206=DIRECTION('',(-0.5,0.866025403784439,0.));
#6207=DIRECTION('',(0.,0.,1.));
#6208=DIRECTION('',(0.,1.,0.));
#6209=DIRECTION('',(0.,0.,1.));
#6210=DIRECTION('',(0.,1.,0.));
#6211=DIRECTION('',(0.,0.,1.));
#6212=DIRECTION('',(0.,1.,0.));
#6213=DIRECTION('',(0.,0.,1.));
#6214=DIRECTION('',(0.,1.,0.));
#6215=DIRECTION('',(0.,0.,1.));
#6216=DIRECTION('',(0.,1.,0.));
#6217=DIRECTION('',(0.,0.,1.));
#6218=DIRECTION('',(0.,1.,0.));
#6219=DIRECTION('',(0.,0.,1.));
#6220=DIRECTION('',(0.,1.,0.));
#6221=DIRECTION('',(0.,0.,1.));
#6222=DIRECTION('',(0.,1.,0.));
#6223=DIRECTION('',(0.,0.,1.));
#6224=DIRECTION('',(-1.,6.12323399573677E-17,0.));
#6225=DIRECTION('',(0.,0.,1.));
#6226=DIRECTION('',(-1.,6.12323399573677E-17,0.));
#6227=DIRECTION('',(0.,0.,1.));
#6228=DIRECTION('',(0.,1.,0.));
#6229=DIRECTION('',(0.,0.,1.));
#6230=DIRECTION('',(0.,1.,0.));
#6231=DIRECTION('',(0.,0.,1.));
#6232=CARTESIAN_POINT('',(0.,0.,0.));
#6233=CARTESIAN_POINT('',(0.,0.,0.));
#6234=CARTESIAN_POINT('Origin',(65.75,0.,0.));
#6235=CARTESIAN_POINT('',(65.2272111655667,11.05,-4.81623674987417E-16));
#6236=CARTESIAN_POINT('',(65.2272111655668,-11.0491603167577,0.000511766293852513));
#6237=CARTESIAN_POINT('Ctrl Pts',(65.2272111655667,11.05,-8.04843840616275E-16));
#6238=CARTESIAN_POINT('Ctrl Pts',(65.2272111655667,11.05,1.65300226112955));
#6239=CARTESIAN_POINT('Ctrl Pts',(65.2272111655667,10.6732111658624,3.30528105206125));
#6240=CARTESIAN_POINT('Ctrl Pts',(65.2272111655667,9.95613525638491,4.79448116918521));
#6241=CARTESIAN_POINT('Ctrl Pts',(65.2272111655667,9.2390593469074,6.28368128630917));
#6242=CARTESIAN_POINT('Ctrl Pts',(65.2272111655667,8.18169636208996,7.60980272962538));
#6243=CARTESIAN_POINT('Ctrl Pts',(65.2272111655667,6.88961460043875,8.63998814917286));
#6244=CARTESIAN_POINT('Ctrl Pts',(65.2272111655667,5.59753283878755,9.67017356872034));
#6245=CARTESIAN_POINT('Ctrl Pts',(65.2272111655667,4.07073230030258,10.4044229644991));
#6246=CARTESIAN_POINT('Ctrl Pts',(65.2272111655667,2.45913707576071,10.7727896191196));
#6247=CARTESIAN_POINT('Ctrl Pts',(65.2272111655667,0.847541851218851,11.14115627374));
#6248=CARTESIAN_POINT('Ctrl Pts',(65.2272111655667,-0.848848059379907,11.1436401872022));
#6249=CARTESIAN_POINT('Ctrl Pts',(65.2272111655667,-2.45957472900739,10.7749338027229));
#6250=CARTESIAN_POINT('Ctrl Pts',(65.2272111655667,-4.6072102885107,10.2833252900838));
#6251=CARTESIAN_POINT('Ctrl Pts',(65.2272111655668,-6.60255564184286,9.13182291443765));
#6252=CARTESIAN_POINT('Ctrl Pts',(65.2272111655667,-8.10144894371101,7.51774250750075));
#6253=CARTESIAN_POINT('Ctrl Pts',(65.2272111655667,-8.85089559464509,6.7107023040323));
#6254=CARTESIAN_POINT('Ctrl Pts',(65.2272111655667,-9.47622923271317,5.78801759274117));
#6255=CARTESIAN_POINT('Ctrl Pts',(65.2272111655667,-9.95481493068238,4.79417459098899));
#6256=CARTESIAN_POINT('Ctrl Pts',(65.2272111655667,-10.4334006286516,3.80033158923682));
#6257=CARTESIAN_POINT('Ctrl Pts',(65.2272111655667,-10.7652383865219,2.7353302970236));
#6258=CARTESIAN_POINT('Ctrl Pts',(65.2272111655667,-10.9288653221363,1.64620606893596));
#6259=CARTESIAN_POINT('Ctrl Pts',(65.2272111655667,-11.0106742828143,1.10167395498666));
#6260=CARTESIAN_POINT('Ctrl Pts',(65.2272111655667,-11.0504351711937,0.551111771520428));
#6261=CARTESIAN_POINT('Ctrl Pts',(65.2272111655667,-11.0491603167577,0.000511766293852513));
#6262=CARTESIAN_POINT('Ctrl Pts',(65.2272111655668,-11.0491603167577,0.000511766293852513));
#6263=CARTESIAN_POINT('Ctrl Pts',(65.2272111655667,-11.0453354725056,-1.6514095869656));
#6264=CARTESIAN_POINT('Ctrl Pts',(65.2272111655667,-10.6721346818115,-3.30367138607943));
#6265=CARTESIAN_POINT('Ctrl Pts',(65.2272111655667,-9.95689686460624,-4.79444728464091));
#6266=CARTESIAN_POINT('Ctrl Pts',(65.2272111655667,-9.48008040912453,-5.78827963350521));
#6267=CARTESIAN_POINT('Ctrl Pts',(65.2272111655667,-8.85125308035079,-6.71034310688341));
#6268=CARTESIAN_POINT('Ctrl Pts',(65.2272111655667,-8.1003801793731,-7.51685624327848));
#6269=CARTESIAN_POINT('Ctrl Pts',(65.2272111655667,-6.59863437741774,-9.12988251606863));
#6270=CARTESIAN_POINT('Ctrl Pts',(65.2272111655667,-4.60870628664658,-10.2807074409263));
#6271=CARTESIAN_POINT('Ctrl Pts',(65.2272111655667,-2.46069090561872,-10.7753211533687));
#6272=CARTESIAN_POINT('Ctrl Pts',(65.2272111655667,-1.38668321510479,-11.0226280095899));
#6273=CARTESIAN_POINT('Ctrl Pts',(65.2272111655667,-0.273153702026687,-11.1058820627073));
#6274=CARTESIAN_POINT('Ctrl Pts',(65.2272111655667,0.826207461938887,-11.0215937869587));
#6275=CARTESIAN_POINT('Ctrl Pts',(65.2272111655668,3.02492978987003,-10.8530172354614));
#6276=CARTESIAN_POINT('Ctrl Pts',(65.2272111655668,5.16697872135103,-10.0142713685));
#6277=CARTESIAN_POINT('Ctrl Pts',(65.2272111655668,6.89007612693015,-8.64177550465633));
#6278=CARTESIAN_POINT('Ctrl Pts',(65.2272111655668,8.1823991811145,-7.61240360677354));
#6279=CARTESIAN_POINT('Ctrl Pts',(65.2272111655667,9.23906200197904,-6.28279733564443));
#6280=CARTESIAN_POINT('Ctrl Pts',(65.2272111655667,9.95596220670041,-4.79294699923343));
#6281=CARTESIAN_POINT('Ctrl Pts',(65.2272111655667,10.6728624114218,-3.30309666282243));
#6282=CARTESIAN_POINT('Ctrl Pts',(65.2272111655667,11.05,-1.65300226112955));
#6283=CARTESIAN_POINT('Ctrl Pts',(65.2272111655667,11.05,-1.11022302462423E-15));
#6284=CARTESIAN_POINT('',(66.717944947177,-11.05,1.35323471305783E-15));
#6285=CARTESIAN_POINT('',(65.75,-11.05,-1.35323471305783E-15));
#6286=CARTESIAN_POINT('',(66.717944947177,-1.35323471305783E-15,11.05));
#6287=CARTESIAN_POINT('Origin',(66.717944947177,0.,0.));
#6288=CARTESIAN_POINT('Origin',(66.717944947177,0.,0.));
#6289=CARTESIAN_POINT('Ctrl Pts',(65.2272111655675,11.0499999999996,-8.04843840616481E-16));
#6290=CARTESIAN_POINT('Ctrl Pts',(65.2272111655675,11.0499999999996,1.65300226112949));
#6291=CARTESIAN_POINT('Ctrl Pts',(65.2272111655675,10.2964223317245,4.95755984299279));
#6292=CARTESIAN_POINT('Ctrl Pts',(65.2272111655675,7.12433337727229,8.9359241729413));
#6293=CARTESIAN_POINT('Ctrl Pts',(65.2272111655675,2.54393176181752,11.1386723602775));
#6294=CARTESIAN_POINT('Ctrl Pts',(65.2272111655675,-3.11070127351147,11.1469520718181));
#6295=CARTESIAN_POINT('Ctrl Pts',(65.2272111655675,-7.60022831850869,8.55607172661427));
#6296=CARTESIAN_POINT('Ctrl Pts',(65.2272111655675,-10.1015628707809,4.86533288144987));
#6297=CARTESIAN_POINT('Ctrl Pts',(65.2272111655675,-11.4289139022623,0.605327712597159));
#6298=CARTESIAN_POINT('Ctrl Pts',(65.2272111655675,-10.7377350666716,-3.94415268674868));
#6299=CARTESIAN_POINT('Ctrl Pts',(65.2272111655675,-7.59359842280306,-8.55447005363952));
#6300=CARTESIAN_POINT('Ctrl Pts',(65.2272111655675,-3.61374224126088,-10.8561199033547));
#6301=CARTESIAN_POINT('Ctrl Pts',(65.2272111655675,1.95390532412946,-11.2723901689417));
#6302=CARTESIAN_POINT('Ctrl Pts',(65.2272111655675,6.77351541996157,-9.3852119682787));
#6303=CARTESIAN_POINT('Ctrl Pts',(65.2272111655675,10.2957248228432,-4.95319106451515));
#6304=CARTESIAN_POINT('Ctrl Pts',(65.2272111655675,11.0499999999996,-1.65300226112949));
#6305=CARTESIAN_POINT('Ctrl Pts',(65.2272111655675,11.0499999999996,-1.40162863026563E-15));
#6306=CARTESIAN_POINT('Ctrl Pts',(65.0809549842406,11.1208351015851,-7.65476926691726E-16));
#6307=CARTESIAN_POINT('Ctrl Pts',(65.0809549842406,11.1208351015851,1.66346926418635));
#6308=CARTESIAN_POINT('Ctrl Pts',(65.0809549842406,10.3623404117656,4.98933947213189));
#6309=CARTESIAN_POINT('Ctrl Pts',(65.0809549842406,7.16993389260531,8.99309464113236));
#6310=CARTESIAN_POINT('Ctrl Pts',(65.0809549842406,2.5601655446675,11.2100133239775));
#6311=CARTESIAN_POINT('Ctrl Pts',(65.0809549842406,-3.1306002334161,11.2182832653346));
#6312=CARTESIAN_POINT('Ctrl Pts',(65.0809549842406,-7.64889972369121,8.61085072005576));
#6313=CARTESIAN_POINT('Ctrl Pts',(65.0809549842406,-10.1662171602437,4.89646684843357));
#6314=CARTESIAN_POINT('Ctrl Pts',(65.0809549842406,-11.5020966787491,0.609220450083247));
#6315=CARTESIAN_POINT('Ctrl Pts',(65.0809549842406,-10.8064244099587,-3.96945703932799));
#6316=CARTESIAN_POINT('Ctrl Pts',(65.0809549842406,-7.64230494153489,-8.60917577599024));
#6317=CARTESIAN_POINT('Ctrl Pts',(65.0809549842406,-3.63683147635714,-10.9256030117343));
#6318=CARTESIAN_POINT('Ctrl Pts',(65.0809549842406,1.96642553185435,-11.3445597508395));
#6319=CARTESIAN_POINT('Ctrl Pts',(65.0809549842406,6.81683558342508,-9.44530445284557));
#6320=CARTESIAN_POINT('Ctrl Pts',(65.0809549842406,10.361637717681,-4.98493807774593));
#6321=CARTESIAN_POINT('Ctrl Pts',(65.0809549842406,11.1208351015851,-1.66346926418635));
#6322=CARTESIAN_POINT('Ctrl Pts',(65.0809549842406,11.1208351015851,-1.22466367006471E-15));
#6323=CARTESIAN_POINT('Ctrl Pts',(64.9738208717935,11.26708032966,-6.84261163180322E-16));
#6324=CARTESIAN_POINT('Ctrl Pts',(64.9738208717935,11.26708032966,1.68537120997538));
#6325=CARTESIAN_POINT('Ctrl Pts',(64.9738208717935,10.4986285999894,5.05495216898997));
#6326=CARTESIAN_POINT('Ctrl Pts',(64.9738208717935,7.26423670697669,9.11138183115333));
#6327=CARTESIAN_POINT('Ctrl Pts',(64.9738208717935,2.59384822348416,11.3574440526352));
#6328=CARTESIAN_POINT('Ctrl Pts',(64.9738208717935,-3.17177793453904,11.3658355627214));
#6329=CARTESIAN_POINT('Ctrl Pts',(64.9738208717935,-7.74949708797367,8.72410231053509));
#6330=CARTESIAN_POINT('Ctrl Pts',(64.9738208717935,-10.299929206767,4.96086932020551));
#6331=CARTESIAN_POINT('Ctrl Pts',(64.9738208717935,-11.6533722919867,0.617229526149155));
#6332=CARTESIAN_POINT('Ctrl Pts',(64.9738208717935,-10.9485643243391,-4.0216534100572));
#6333=CARTESIAN_POINT('Ctrl Pts',(64.9738208717935,-7.74279975532283,-8.72241818640559));
#6334=CARTESIAN_POINT('Ctrl Pts',(64.9738208717935,-3.68467342228032,-11.0693030819176));
#6335=CARTESIAN_POINT('Ctrl Pts',(64.9738208717935,1.99228617997655,-11.4937656657012));
#6336=CARTESIAN_POINT('Ctrl Pts',(64.9738208717935,6.90650137190516,-9.56952991364493));
#6337=CARTESIAN_POINT('Ctrl Pts',(64.9738208717935,10.4979168106424,-5.05049383381464));
#6338=CARTESIAN_POINT('Ctrl Pts',(64.9738208717935,11.26708032966,-1.68537120997538));
#6339=CARTESIAN_POINT('Ctrl Pts',(64.9738208717935,11.26708032966,-8.59329092798487E-16));
#6340=CARTESIAN_POINT('Ctrl Pts',(64.9503835492166,11.4278882091416,-5.94987561328448E-16));
#6341=CARTESIAN_POINT('Ctrl Pts',(64.9503835492166,11.4278882091416,1.70953167870107));
#6342=CARTESIAN_POINT('Ctrl Pts',(64.9503835492166,10.6485396706842,5.12709861319939));
#6343=CARTESIAN_POINT('Ctrl Pts',(64.9503835492166,7.36797152942324,9.24151515780478));
#6344=CARTESIAN_POINT('Ctrl Pts',(64.9503835492167,2.63092921137885,11.519592989277));
#6345=CARTESIAN_POINT('Ctrl Pts',(64.9503835492166,-3.21708112269002,11.5281558506245));
#6346=CARTESIAN_POINT('Ctrl Pts',(64.9503835492167,-7.86014113917398,8.84867250689127));
#6347=CARTESIAN_POINT('Ctrl Pts',(64.9503835492167,-10.4470164004438,5.03171767144541));
#6348=CARTESIAN_POINT('Ctrl Pts',(64.9503835492166,-11.8197602196346,0.6260287266476));
#6349=CARTESIAN_POINT('Ctrl Pts',(64.9503835492166,-11.1049444308876,-4.0790349306743));
#6350=CARTESIAN_POINT('Ctrl Pts',(64.9503835492167,-7.85328451410953,-8.84701605985931));
#6351=CARTESIAN_POINT('Ctrl Pts',(64.9503835492166,-3.73732509952793,-11.2273777955275));
#6352=CARTESIAN_POINT('Ctrl Pts',(64.9503835492166,2.02072503306777,-11.6578836833029));
#6353=CARTESIAN_POINT('Ctrl Pts',(64.9503835492167,7.0051562897937,-9.7061677097367));
#6354=CARTESIAN_POINT('Ctrl Pts',(64.9503835492166,10.6478183083747,-5.12258043111314));
#6355=CARTESIAN_POINT('Ctrl Pts',(64.9503835492167,11.4278882091416,-1.70953167870107));
#6356=CARTESIAN_POINT('Ctrl Pts',(64.9503835492167,11.4278882091416,-4.57627715103496E-16));
#6357=CARTESIAN_POINT('',(64.9503835492166,11.4278882091416,1.38777878078145E-16));
#6358=CARTESIAN_POINT('Origin',(65.4451561127438,11.5,-5.55111512312578E-16));
#6359=CARTESIAN_POINT('Ctrl Pts',(64.9503835492167,11.4278882091416,-4.57627715103496E-16));
#6360=CARTESIAN_POINT('Ctrl Pts',(64.9503835492167,11.4278882091416,-1.70953167870107));
#6361=CARTESIAN_POINT('Ctrl Pts',(64.9503835492166,10.6478183083747,-5.12258043111314));
#6362=CARTESIAN_POINT('Ctrl Pts',(64.9503835492167,7.0051562897937,-9.7061677097367));
#6363=CARTESIAN_POINT('Ctrl Pts',(64.9503835492166,2.02072503306777,-11.6578836833029));
#6364=CARTESIAN_POINT('Ctrl Pts',(64.9503835492166,-3.73732509952793,-11.2273777955275));
#6365=CARTESIAN_POINT('Ctrl Pts',(64.9503835492167,-7.85328451410953,-8.84701605985931));
#6366=CARTESIAN_POINT('Ctrl Pts',(64.9503835492166,-11.1049444308876,-4.0790349306743));
#6367=CARTESIAN_POINT('Ctrl Pts',(64.9503835492166,-11.8197602196346,0.6260287266476));
#6368=CARTESIAN_POINT('Ctrl Pts',(64.9503835492167,-10.4470164004438,5.03171767144541));
#6369=CARTESIAN_POINT('Ctrl Pts',(64.9503835492167,-7.86014113917398,8.84867250689127));
#6370=CARTESIAN_POINT('Ctrl Pts',(64.9503835492166,-3.21708112269002,11.5281558506245));
#6371=CARTESIAN_POINT('Ctrl Pts',(64.9503835492167,2.63092921137885,11.519592989277));
#6372=CARTESIAN_POINT('Ctrl Pts',(64.9503835492166,7.36797152942324,9.24151515780478));
#6373=CARTESIAN_POINT('Ctrl Pts',(64.9503835492166,10.6485396706842,5.12709861319939));
#6374=CARTESIAN_POINT('Ctrl Pts',(64.9503835492166,11.4278882091416,1.70953167870107));
#6375=CARTESIAN_POINT('Ctrl Pts',(64.9503835492166,11.4278882091416,-5.94987561328448E-16));
#6376=CARTESIAN_POINT('Ctrl Pts',(58.1,25.5,0.));
#6377=CARTESIAN_POINT('Ctrl Pts',(58.1,25.5,25.5));
#6378=CARTESIAN_POINT('Ctrl Pts',(58.1,0.,25.5));
#6379=CARTESIAN_POINT('Ctrl Pts',(58.1,-25.5,25.5));
#6380=CARTESIAN_POINT('Ctrl Pts',(58.1,-25.5,0.));
#6381=CARTESIAN_POINT('Ctrl Pts',(58.1,-25.5,-25.5));
#6382=CARTESIAN_POINT('Ctrl Pts',(58.1,0.,-25.5));
#6383=CARTESIAN_POINT('Ctrl Pts',(58.1,25.5,-25.5));
#6384=CARTESIAN_POINT('Ctrl Pts',(58.1,25.5,0.));
#6385=CARTESIAN_POINT('Ctrl Pts',(58.1006850861903,25.3693230990265,0.));
#6386=CARTESIAN_POINT('Ctrl Pts',(58.1006850861903,25.3693230990265,25.3693230990265));
#6387=CARTESIAN_POINT('Ctrl Pts',(58.1006850861903,0.,25.3693230990265));
#6388=CARTESIAN_POINT('Ctrl Pts',(58.1006850861903,-25.3693230990265,25.3693230990265));
#6389=CARTESIAN_POINT('Ctrl Pts',(58.1006850861903,-25.3693230990265,0.));
#6390=CARTESIAN_POINT('Ctrl Pts',(58.1006850861903,-25.3693230990265,-25.3693230990265));
#6391=CARTESIAN_POINT('Ctrl Pts',(58.1006850861903,0.,-25.3693230990265));
#6392=CARTESIAN_POINT('Ctrl Pts',(58.1006850861903,25.3693230990265,-25.3693230990265));
#6393=CARTESIAN_POINT('Ctrl Pts',(58.1006850861903,25.3693230990265,0.));
#6394=CARTESIAN_POINT('Ctrl Pts',(58.106842887577,25.1090017061965,0.));
#6395=CARTESIAN_POINT('Ctrl Pts',(58.106842887577,25.1090017061965,25.1090017061965));
#6396=CARTESIAN_POINT('Ctrl Pts',(58.106842887577,0.,25.1090017061965));
#6397=CARTESIAN_POINT('Ctrl Pts',(58.106842887577,-25.1090017061965,25.1090017061965));
#6398=CARTESIAN_POINT('Ctrl Pts',(58.106842887577,-25.1090017061965,0.));
#6399=CARTESIAN_POINT('Ctrl Pts',(58.106842887577,-25.1090017061965,-25.1090017061965));
#6400=CARTESIAN_POINT('Ctrl Pts',(58.106842887577,0.,-25.1090017061965));
#6401=CARTESIAN_POINT('Ctrl Pts',(58.106842887577,25.1090017061965,-25.1090017061965));
#6402=CARTESIAN_POINT('Ctrl Pts',(58.106842887577,25.1090017061965,0.));
#6403=CARTESIAN_POINT('Ctrl Pts',(58.1304424850882,24.7216168481987,0.));
#6404=CARTESIAN_POINT('Ctrl Pts',(58.1304424850882,24.7216168481987,24.7216168481987));
#6405=CARTESIAN_POINT('Ctrl Pts',(58.1304424850882,0.,24.7216168481987));
#6406=CARTESIAN_POINT('Ctrl Pts',(58.1304424850882,-24.7216168481987,24.7216168481987));
#6407=CARTESIAN_POINT('Ctrl Pts',(58.1304424850882,-24.7216168481987,0.));
#6408=CARTESIAN_POINT('Ctrl Pts',(58.1304424850882,-24.7216168481987,-24.7216168481987));
#6409=CARTESIAN_POINT('Ctrl Pts',(58.1304424850882,0.,-24.7216168481987));
#6410=CARTESIAN_POINT('Ctrl Pts',(58.1304424850882,24.7216168481987,-24.7216168481987));
#6411=CARTESIAN_POINT('Ctrl Pts',(58.1304424850882,24.7216168481987,0.));
#6412=CARTESIAN_POINT('Ctrl Pts',(58.1907092774481,24.2113142943935,0.));
#6413=CARTESIAN_POINT('Ctrl Pts',(58.1907092774481,24.2113142943935,24.2113142943935));
#6414=CARTESIAN_POINT('Ctrl Pts',(58.1907092774481,0.,24.2113142943935));
#6415=CARTESIAN_POINT('Ctrl Pts',(58.1907092774481,-24.2113142943935,24.2113142943935));
#6416=CARTESIAN_POINT('Ctrl Pts',(58.1907092774481,-24.2113142943935,0.));
#6417=CARTESIAN_POINT('Ctrl Pts',(58.1907092774481,-24.2113142943935,-24.2113142943935));
#6418=CARTESIAN_POINT('Ctrl Pts',(58.1907092774481,0.,-24.2113142943935));
#6419=CARTESIAN_POINT('Ctrl Pts',(58.1907092774481,24.2113142943935,-24.2113142943935));
#6420=CARTESIAN_POINT('Ctrl Pts',(58.1907092774481,24.2113142943935,0.));
#6421=CARTESIAN_POINT('Ctrl Pts',(58.3142240203109,23.5838111702086,0.));
#6422=CARTESIAN_POINT('Ctrl Pts',(58.3142240203109,23.5838111702086,23.5838111702086));
#6423=CARTESIAN_POINT('Ctrl Pts',(58.3142240203109,0.,23.5838111702086));
#6424=CARTESIAN_POINT('Ctrl Pts',(58.3142240203109,-23.5838111702086,23.5838111702086));
#6425=CARTESIAN_POINT('Ctrl Pts',(58.3142240203109,-23.5838111702086,0.));
#6426=CARTESIAN_POINT('Ctrl Pts',(58.3142240203109,-23.5838111702086,-23.5838111702086));
#6427=CARTESIAN_POINT('Ctrl Pts',(58.3142240203109,0.,-23.5838111702086));
#6428=CARTESIAN_POINT('Ctrl Pts',(58.3142240203109,23.5838111702086,-23.5838111702086));
#6429=CARTESIAN_POINT('Ctrl Pts',(58.3142240203109,23.5838111702086,0.));
#6430=CARTESIAN_POINT('Ctrl Pts',(58.4856917608691,22.9665891529976,0.));
#6431=CARTESIAN_POINT('Ctrl Pts',(58.4856917608691,22.9665891529976,22.9665891529976));
#6432=CARTESIAN_POINT('Ctrl Pts',(58.4856917608691,0.,22.9665891529976));
#6433=CARTESIAN_POINT('Ctrl Pts',(58.4856917608691,-22.9665891529976,22.9665891529976));
#6434=CARTESIAN_POINT('Ctrl Pts',(58.4856917608691,-22.9665891529976,0.));
#6435=CARTESIAN_POINT('Ctrl Pts',(58.4856917608691,-22.9665891529976,-22.9665891529976));
#6436=CARTESIAN_POINT('Ctrl Pts',(58.4856917608691,0.,-22.9665891529976));
#6437=CARTESIAN_POINT('Ctrl Pts',(58.4856917608691,22.9665891529976,-22.9665891529976));
#6438=CARTESIAN_POINT('Ctrl Pts',(58.4856917608691,22.9665891529976,0.));
#6439=CARTESIAN_POINT('Ctrl Pts',(58.7040649536582,22.3593331170216,0.));
#6440=CARTESIAN_POINT('Ctrl Pts',(58.7040649536582,22.3593331170216,22.3593331170216));
#6441=CARTESIAN_POINT('Ctrl Pts',(58.7040649536582,0.,22.3593331170216));
#6442=CARTESIAN_POINT('Ctrl Pts',(58.7040649536582,-22.3593331170216,22.3593331170216));
#6443=CARTESIAN_POINT('Ctrl Pts',(58.7040649536582,-22.3593331170216,0.));
#6444=CARTESIAN_POINT('Ctrl Pts',(58.7040649536582,-22.3593331170216,-22.3593331170216));
#6445=CARTESIAN_POINT('Ctrl Pts',(58.7040649536582,0.,-22.3593331170216));
#6446=CARTESIAN_POINT('Ctrl Pts',(58.7040649536582,22.3593331170216,-22.3593331170216));
#6447=CARTESIAN_POINT('Ctrl Pts',(58.7040649536582,22.3593331170216,0.));
#6448=CARTESIAN_POINT('Ctrl Pts',(58.9670233800433,21.7613919711372,0.));
#6449=CARTESIAN_POINT('Ctrl Pts',(58.9670233800433,21.7613919711372,21.7613919711372));
#6450=CARTESIAN_POINT('Ctrl Pts',(58.9670233800433,0.,21.7613919711372));
#6451=CARTESIAN_POINT('Ctrl Pts',(58.9670233800433,-21.7613919711372,21.7613919711372));
#6452=CARTESIAN_POINT('Ctrl Pts',(58.9670233800433,-21.7613919711372,0.));
#6453=CARTESIAN_POINT('Ctrl Pts',(58.9670233800433,-21.7613919711372,-21.7613919711372));
#6454=CARTESIAN_POINT('Ctrl Pts',(58.9670233800433,0.,-21.7613919711372));
#6455=CARTESIAN_POINT('Ctrl Pts',(58.9670233800433,21.7613919711372,-21.7613919711372));
#6456=CARTESIAN_POINT('Ctrl Pts',(58.9670233800433,21.7613919711372,0.));
#6457=CARTESIAN_POINT('Ctrl Pts',(59.2705528391893,21.1716763589853,0.));
#6458=CARTESIAN_POINT('Ctrl Pts',(59.2705528391893,21.1716763589853,21.1716763589853));
#6459=CARTESIAN_POINT('Ctrl Pts',(59.2705528391893,0.,21.1716763589853));
#6460=CARTESIAN_POINT('Ctrl Pts',(59.2705528391893,-21.1716763589853,21.1716763589853));
#6461=CARTESIAN_POINT('Ctrl Pts',(59.2705528391893,-21.1716763589853,0.));
#6462=CARTESIAN_POINT('Ctrl Pts',(59.2705528391893,-21.1716763589853,-21.1716763589853));
#6463=CARTESIAN_POINT('Ctrl Pts',(59.2705528391893,0.,-21.1716763589853));
#6464=CARTESIAN_POINT('Ctrl Pts',(59.2705528391893,21.1716763589853,-21.1716763589853));
#6465=CARTESIAN_POINT('Ctrl Pts',(59.2705528391893,21.1716763589853,0.));
#6466=CARTESIAN_POINT('Ctrl Pts',(59.6094227136446,20.5888495299376,0.));
#6467=CARTESIAN_POINT('Ctrl Pts',(59.6094227136446,20.5888495299376,20.5888495299376));
#6468=CARTESIAN_POINT('Ctrl Pts',(59.6094227136446,0.,20.5888495299376));
#6469=CARTESIAN_POINT('Ctrl Pts',(59.6094227136446,-20.5888495299376,20.5888495299376));
#6470=CARTESIAN_POINT('Ctrl Pts',(59.6094227136446,-20.5888495299376,0.));
#6471=CARTESIAN_POINT('Ctrl Pts',(59.6094227136446,-20.5888495299376,-20.5888495299376));
#6472=CARTESIAN_POINT('Ctrl Pts',(59.6094227136446,0.,-20.5888495299376));
#6473=CARTESIAN_POINT('Ctrl Pts',(59.6094227136446,20.5888495299376,-20.5888495299376));
#6474=CARTESIAN_POINT('Ctrl Pts',(59.6094227136446,20.5888495299376,0.));
#6475=CARTESIAN_POINT('Ctrl Pts',(59.9775897880897,20.0114964775053,0.));
#6476=CARTESIAN_POINT('Ctrl Pts',(59.9775897880897,20.0114964775053,20.0114964775053));
#6477=CARTESIAN_POINT('Ctrl Pts',(59.9775897880897,0.,20.0114964775053));
#6478=CARTESIAN_POINT('Ctrl Pts',(59.9775897880897,-20.0114964775053,20.0114964775053));
#6479=CARTESIAN_POINT('Ctrl Pts',(59.9775897880897,-20.0114964775053,0.));
#6480=CARTESIAN_POINT('Ctrl Pts',(59.9775897880897,-20.0114964775053,-20.0114964775053));
#6481=CARTESIAN_POINT('Ctrl Pts',(59.9775897880897,0.,-20.0114964775053));
#6482=CARTESIAN_POINT('Ctrl Pts',(59.9775897880897,20.0114964775053,-20.0114964775053));
#6483=CARTESIAN_POINT('Ctrl Pts',(59.9775897880897,20.0114964775053,0.));
#6484=CARTESIAN_POINT('Ctrl Pts',(60.3686078898803,19.4382992332324,0.));
#6485=CARTESIAN_POINT('Ctrl Pts',(60.3686078898803,19.4382992332324,19.4382992332324));
#6486=CARTESIAN_POINT('Ctrl Pts',(60.3686078898803,0.,19.4382992332324));
#6487=CARTESIAN_POINT('Ctrl Pts',(60.3686078898803,-19.4382992332324,19.4382992332324));
#6488=CARTESIAN_POINT('Ctrl Pts',(60.3686078898803,-19.4382992332324,0.));
#6489=CARTESIAN_POINT('Ctrl Pts',(60.3686078898803,-19.4382992332324,-19.4382992332324));
#6490=CARTESIAN_POINT('Ctrl Pts',(60.3686078898803,0.,-19.4382992332324));
#6491=CARTESIAN_POINT('Ctrl Pts',(60.3686078898803,19.4382992332324,-19.4382992332324));
#6492=CARTESIAN_POINT('Ctrl Pts',(60.3686078898803,19.4382992332324,0.));
#6493=CARTESIAN_POINT('Ctrl Pts',(60.7760056975964,18.8682016392444,0.));
#6494=CARTESIAN_POINT('Ctrl Pts',(60.7760056975964,18.8682016392444,18.8682016392444));
#6495=CARTESIAN_POINT('Ctrl Pts',(60.7760056975964,0.,18.8682016392444));
#6496=CARTESIAN_POINT('Ctrl Pts',(60.7760056975964,-18.8682016392444,18.8682016392444));
#6497=CARTESIAN_POINT('Ctrl Pts',(60.7760056975964,-18.8682016392444,0.));
#6498=CARTESIAN_POINT('Ctrl Pts',(60.7760056975964,-18.8682016392444,-18.8682016392444));
#6499=CARTESIAN_POINT('Ctrl Pts',(60.7760056975964,0.,-18.8682016392444));
#6500=CARTESIAN_POINT('Ctrl Pts',(60.7760056975964,18.8682016392444,-18.8682016392444));
#6501=CARTESIAN_POINT('Ctrl Pts',(60.7760056975964,18.8682016392444,0.));
#6502=CARTESIAN_POINT('Ctrl Pts',(61.1936904784186,18.3005942681782,0.));
#6503=CARTESIAN_POINT('Ctrl Pts',(61.1936904784186,18.3005942681782,18.3005942681782));
#6504=CARTESIAN_POINT('Ctrl Pts',(61.1936904784186,0.,18.3005942681782));
#6505=CARTESIAN_POINT('Ctrl Pts',(61.1936904784186,-18.3005942681782,18.3005942681782));
#6506=CARTESIAN_POINT('Ctrl Pts',(61.1936904784186,-18.3005942681782,0.));
#6507=CARTESIAN_POINT('Ctrl Pts',(61.1936904784186,-18.3005942681782,-18.3005942681782));
#6508=CARTESIAN_POINT('Ctrl Pts',(61.1936904784186,0.,-18.3005942681782));
#6509=CARTESIAN_POINT('Ctrl Pts',(61.1936904784186,18.3005942681782,-18.3005942681782));
#6510=CARTESIAN_POINT('Ctrl Pts',(61.1936904784186,18.3005942681782,0.));
#6511=CARTESIAN_POINT('Ctrl Pts',(61.6158386260792,17.7351881055358,0.));
#6512=CARTESIAN_POINT('Ctrl Pts',(61.6158386260792,17.7351881055358,17.7351881055358));
#6513=CARTESIAN_POINT('Ctrl Pts',(61.6158386260792,0.,17.7351881055358));
#6514=CARTESIAN_POINT('Ctrl Pts',(61.6158386260792,-17.7351881055358,17.7351881055358));
#6515=CARTESIAN_POINT('Ctrl Pts',(61.6158386260792,-17.7351881055358,0.));
#6516=CARTESIAN_POINT('Ctrl Pts',(61.6158386260792,-17.7351881055358,-17.7351881055358));
#6517=CARTESIAN_POINT('Ctrl Pts',(61.6158386260792,0.,-17.7351881055358));
#6518=CARTESIAN_POINT('Ctrl Pts',(61.6158386260792,17.7351881055358,-17.7351881055358));
#6519=CARTESIAN_POINT('Ctrl Pts',(61.6158386260792,17.7351881055358,0.));
#6520=CARTESIAN_POINT('Ctrl Pts',(62.0367583558289,17.1718725504246,0.));
#6521=CARTESIAN_POINT('Ctrl Pts',(62.0367583558289,17.1718725504246,17.1718725504246));
#6522=CARTESIAN_POINT('Ctrl Pts',(62.0367583558289,0.,17.1718725504246));
#6523=CARTESIAN_POINT('Ctrl Pts',(62.0367583558289,-17.1718725504246,17.1718725504246));
#6524=CARTESIAN_POINT('Ctrl Pts',(62.0367583558289,-17.1718725504246,0.));
#6525=CARTESIAN_POINT('Ctrl Pts',(62.0367583558289,-17.1718725504246,-17.1718725504246));
#6526=CARTESIAN_POINT('Ctrl Pts',(62.0367583558289,0.,-17.1718725504246));
#6527=CARTESIAN_POINT('Ctrl Pts',(62.0367583558289,17.1718725504246,-17.1718725504246));
#6528=CARTESIAN_POINT('Ctrl Pts',(62.0367583558289,17.1718725504246,0.));
#6529=CARTESIAN_POINT('Ctrl Pts',(62.4507485326533,16.6105738821721,0.));
#6530=CARTESIAN_POINT('Ctrl Pts',(62.4507485326533,16.6105738821721,16.6105738821721));
#6531=CARTESIAN_POINT('Ctrl Pts',(62.4507485326533,0.,16.6105738821721));
#6532=CARTESIAN_POINT('Ctrl Pts',(62.4507485326533,-16.6105738821721,16.6105738821721));
#6533=CARTESIAN_POINT('Ctrl Pts',(62.4507485326533,-16.6105738821721,0.));
#6534=CARTESIAN_POINT('Ctrl Pts',(62.4507485326533,-16.6105738821721,-16.6105738821721));
#6535=CARTESIAN_POINT('Ctrl Pts',(62.4507485326533,0.,-16.6105738821721));
#6536=CARTESIAN_POINT('Ctrl Pts',(62.4507485326533,16.6105738821721,-16.6105738821721));
#6537=CARTESIAN_POINT('Ctrl Pts',(62.4507485326533,16.6105738821721,0.));
#6538=CARTESIAN_POINT('Ctrl Pts',(62.8519889360609,16.0511281710465,0.));
#6539=CARTESIAN_POINT('Ctrl Pts',(62.8519889360609,16.0511281710465,16.0511281710465));
#6540=CARTESIAN_POINT('Ctrl Pts',(62.8519889360609,0.,16.0511281710465));
#6541=CARTESIAN_POINT('Ctrl Pts',(62.8519889360609,-16.0511281710465,16.0511281710465));
#6542=CARTESIAN_POINT('Ctrl Pts',(62.8519889360609,-16.0511281710465,0.));
#6543=CARTESIAN_POINT('Ctrl Pts',(62.8519889360609,-16.0511281710465,-16.0511281710465));
#6544=CARTESIAN_POINT('Ctrl Pts',(62.8519889360609,0.,-16.0511281710465));
#6545=CARTESIAN_POINT('Ctrl Pts',(62.8519889360609,16.0511281710465,-16.0511281710465));
#6546=CARTESIAN_POINT('Ctrl Pts',(62.8519889360609,16.0511281710465,0.));
#6547=CARTESIAN_POINT('Ctrl Pts',(63.2343441839831,15.4931095154543,0.));
#6548=CARTESIAN_POINT('Ctrl Pts',(63.2343441839831,15.4931095154543,15.4931095154543));
#6549=CARTESIAN_POINT('Ctrl Pts',(63.2343441839831,0.,15.4931095154543));
#6550=CARTESIAN_POINT('Ctrl Pts',(63.2343441839831,-15.4931095154543,15.4931095154543));
#6551=CARTESIAN_POINT('Ctrl Pts',(63.2343441839831,-15.4931095154543,0.));
#6552=CARTESIAN_POINT('Ctrl Pts',(63.2343441839831,-15.4931095154543,-15.4931095154543));
#6553=CARTESIAN_POINT('Ctrl Pts',(63.2343441839831,0.,-15.4931095154543));
#6554=CARTESIAN_POINT('Ctrl Pts',(63.2343441839831,15.4931095154543,-15.4931095154543));
#6555=CARTESIAN_POINT('Ctrl Pts',(63.2343441839831,15.4931095154543,0.));
#6556=CARTESIAN_POINT('Ctrl Pts',(63.5915578634715,14.9358503082954,0.));
#6557=CARTESIAN_POINT('Ctrl Pts',(63.5915578634715,14.9358503082954,14.9358503082954));
#6558=CARTESIAN_POINT('Ctrl Pts',(63.5915578634715,0.,14.9358503082954));
#6559=CARTESIAN_POINT('Ctrl Pts',(63.5915578634715,-14.9358503082954,14.9358503082954));
#6560=CARTESIAN_POINT('Ctrl Pts',(63.5915578634715,-14.9358503082954,0.));
#6561=CARTESIAN_POINT('Ctrl Pts',(63.5915578634715,-14.9358503082954,-14.9358503082954));
#6562=CARTESIAN_POINT('Ctrl Pts',(63.5915578634715,0.,-14.9358503082954));
#6563=CARTESIAN_POINT('Ctrl Pts',(63.5915578634715,14.9358503082954,-14.9358503082954));
#6564=CARTESIAN_POINT('Ctrl Pts',(63.5915578634715,14.9358503082954,0.));
#6565=CARTESIAN_POINT('Ctrl Pts',(63.9176667121215,14.3785717762628,0.));
#6566=CARTESIAN_POINT('Ctrl Pts',(63.9176667121215,14.3785717762628,14.3785717762628));
#6567=CARTESIAN_POINT('Ctrl Pts',(63.9176667121215,0.,14.3785717762628));
#6568=CARTESIAN_POINT('Ctrl Pts',(63.9176667121215,-14.3785717762628,14.3785717762628));
#6569=CARTESIAN_POINT('Ctrl Pts',(63.9176667121215,-14.3785717762628,0.));
#6570=CARTESIAN_POINT('Ctrl Pts',(63.9176667121215,-14.3785717762628,-14.3785717762628));
#6571=CARTESIAN_POINT('Ctrl Pts',(63.9176667121215,0.,-14.3785717762628));
#6572=CARTESIAN_POINT('Ctrl Pts',(63.9176667121215,14.3785717762628,-14.3785717762628));
#6573=CARTESIAN_POINT('Ctrl Pts',(63.9176667121215,14.3785717762628,0.));
#6574=CARTESIAN_POINT('Ctrl Pts',(64.2073839217625,13.8204835129561,0.));
#6575=CARTESIAN_POINT('Ctrl Pts',(64.2073839217625,13.8204835129561,13.8204835129561));
#6576=CARTESIAN_POINT('Ctrl Pts',(64.2073839217625,0.,13.8204835129561));
#6577=CARTESIAN_POINT('Ctrl Pts',(64.2073839217625,-13.8204835129561,13.8204835129561));
#6578=CARTESIAN_POINT('Ctrl Pts',(64.2073839217625,-13.8204835129561,0.));
#6579=CARTESIAN_POINT('Ctrl Pts',(64.2073839217625,-13.8204835129561,-13.8204835129561));
#6580=CARTESIAN_POINT('Ctrl Pts',(64.2073839217625,0.,-13.8204835129561));
#6581=CARTESIAN_POINT('Ctrl Pts',(64.2073839217625,13.8204835129561,-13.8204835129561));
#6582=CARTESIAN_POINT('Ctrl Pts',(64.2073839217625,13.8204835129561,0.));
#6583=CARTESIAN_POINT('Ctrl Pts',(64.4564605946371,13.2608853560062,0.));
#6584=CARTESIAN_POINT('Ctrl Pts',(64.4564605946371,13.2608853560062,13.2608853560062));
#6585=CARTESIAN_POINT('Ctrl Pts',(64.4564605946371,0.,13.2608853560062));
#6586=CARTESIAN_POINT('Ctrl Pts',(64.4564605946371,-13.2608853560062,13.2608853560062));
#6587=CARTESIAN_POINT('Ctrl Pts',(64.4564605946371,-13.2608853560062,0.));
#6588=CARTESIAN_POINT('Ctrl Pts',(64.4564605946371,-13.2608853560062,-13.2608853560062));
#6589=CARTESIAN_POINT('Ctrl Pts',(64.4564605946371,0.,-13.2608853560062));
#6590=CARTESIAN_POINT('Ctrl Pts',(64.4564605946371,13.2608853560062,-13.2608853560062));
#6591=CARTESIAN_POINT('Ctrl Pts',(64.4564605946371,13.2608853560062,0.));
#6592=CARTESIAN_POINT('Ctrl Pts',(64.6622177060836,12.6992939860082,0.));
#6593=CARTESIAN_POINT('Ctrl Pts',(64.6622177060836,12.6992939860082,12.6992939860082));
#6594=CARTESIAN_POINT('Ctrl Pts',(64.6622177060836,0.,12.6992939860082));
#6595=CARTESIAN_POINT('Ctrl Pts',(64.6622177060836,-12.6992939860082,12.6992939860082));
#6596=CARTESIAN_POINT('Ctrl Pts',(64.6622177060836,-12.6992939860082,0.));
#6597=CARTESIAN_POINT('Ctrl Pts',(64.6622177060836,-12.6992939860082,-12.6992939860082));
#6598=CARTESIAN_POINT('Ctrl Pts',(64.6622177060836,0.,-12.6992939860082));
#6599=CARTESIAN_POINT('Ctrl Pts',(64.6622177060836,12.6992939860082,-12.6992939860082));
#6600=CARTESIAN_POINT('Ctrl Pts',(64.6622177060836,12.6992939860082,0.));
#6601=CARTESIAN_POINT('Ctrl Pts',(64.8234125059507,12.1354463894458,0.));
#6602=CARTESIAN_POINT('Ctrl Pts',(64.8234125059507,12.1354463894458,12.1354463894458));
#6603=CARTESIAN_POINT('Ctrl Pts',(64.8234125059507,0.,12.1354463894458));
#6604=CARTESIAN_POINT('Ctrl Pts',(64.8234125059507,-12.1354463894458,12.1354463894458));
#6605=CARTESIAN_POINT('Ctrl Pts',(64.8234125059507,-12.1354463894458,0.));
#6606=CARTESIAN_POINT('Ctrl Pts',(64.8234125059507,-12.1354463894458,-12.1354463894458));
#6607=CARTESIAN_POINT('Ctrl Pts',(64.8234125059507,0.,-12.1354463894458));
#6608=CARTESIAN_POINT('Ctrl Pts',(64.8234125059507,12.1354463894458,-12.1354463894458));
#6609=CARTESIAN_POINT('Ctrl Pts',(64.8234125059507,12.1354463894458,0.));
#6610=CARTESIAN_POINT('Ctrl Pts',(64.916430253722,11.6824677271476,0.));
#6611=CARTESIAN_POINT('Ctrl Pts',(64.916430253722,11.6824677271476,11.6824677271476));
#6612=CARTESIAN_POINT('Ctrl Pts',(64.916430253722,0.,11.6824677271476));
#6613=CARTESIAN_POINT('Ctrl Pts',(64.916430253722,-11.6824677271476,11.6824677271476));
#6614=CARTESIAN_POINT('Ctrl Pts',(64.916430253722,-11.6824677271476,0.));
#6615=CARTESIAN_POINT('Ctrl Pts',(64.916430253722,-11.6824677271476,-11.6824677271476));
#6616=CARTESIAN_POINT('Ctrl Pts',(64.916430253722,0.,-11.6824677271476));
#6617=CARTESIAN_POINT('Ctrl Pts',(64.916430253722,11.6824677271476,-11.6824677271476));
#6618=CARTESIAN_POINT('Ctrl Pts',(64.916430253722,11.6824677271476,0.));
#6619=CARTESIAN_POINT('Ctrl Pts',(64.9660346030933,11.3416530788372,0.));
#6620=CARTESIAN_POINT('Ctrl Pts',(64.9660346030933,11.3416530788372,11.3416530788372));
#6621=CARTESIAN_POINT('Ctrl Pts',(64.9660346030933,0.,11.3416530788372));
#6622=CARTESIAN_POINT('Ctrl Pts',(64.9660346030933,-11.3416530788372,11.3416530788372));
#6623=CARTESIAN_POINT('Ctrl Pts',(64.9660346030933,-11.3416530788372,0.));
#6624=CARTESIAN_POINT('Ctrl Pts',(64.9660346030933,-11.3416530788372,-11.3416530788372));
#6625=CARTESIAN_POINT('Ctrl Pts',(64.9660346030933,0.,-11.3416530788372));
#6626=CARTESIAN_POINT('Ctrl Pts',(64.9660346030933,11.3416530788372,-11.3416530788372));
#6627=CARTESIAN_POINT('Ctrl Pts',(64.9660346030933,11.3416530788372,0.));
#6628=CARTESIAN_POINT('Ctrl Pts',(64.9901676141296,11.1139642079645,0.));
#6629=CARTESIAN_POINT('Ctrl Pts',(64.9901676141296,11.1139642079645,11.1139642079645));
#6630=CARTESIAN_POINT('Ctrl Pts',(64.9901676141296,0.,11.1139642079645));
#6631=CARTESIAN_POINT('Ctrl Pts',(64.9901676141296,-11.1139642079645,11.1139642079645));
#6632=CARTESIAN_POINT('Ctrl Pts',(64.9901676141296,-11.1139642079645,0.));
#6633=CARTESIAN_POINT('Ctrl Pts',(64.9901676141296,-11.1139642079645,-11.1139642079645));
#6634=CARTESIAN_POINT('Ctrl Pts',(64.9901676141296,0.,-11.1139642079645));
#6635=CARTESIAN_POINT('Ctrl Pts',(64.9901676141296,11.1139642079645,-11.1139642079645));
#6636=CARTESIAN_POINT('Ctrl Pts',(64.9901676141296,11.1139642079645,0.));
#6637=CARTESIAN_POINT('Ctrl Pts',(65.,11.,0.));
#6638=CARTESIAN_POINT('Ctrl Pts',(65.,11.,11.));
#6639=CARTESIAN_POINT('Ctrl Pts',(65.,0.,11.));
#6640=CARTESIAN_POINT('Ctrl Pts',(65.,-11.,11.));
#6641=CARTESIAN_POINT('Ctrl Pts',(65.,-11.,0.));
#6642=CARTESIAN_POINT('Ctrl Pts',(65.,-11.,-11.));
#6643=CARTESIAN_POINT('Ctrl Pts',(65.,0.,-11.));
#6644=CARTESIAN_POINT('Ctrl Pts',(65.,11.,-11.));
#6645=CARTESIAN_POINT('Ctrl Pts',(65.,11.,0.));
#6646=CARTESIAN_POINT('',(58.1000072797208,25.4986314827274,3.83026943495679E-14));
#6647=CARTESIAN_POINT('Ctrl Pts',(58.1000072797208,25.4986314827274,0.));
#6648=CARTESIAN_POINT('Ctrl Pts',(58.1007109447233,25.3682326055233,0.));
#6649=CARTESIAN_POINT('Ctrl Pts',(58.1068923494636,25.1081903199643,0.));
#6650=CARTESIAN_POINT('Ctrl Pts',(58.1305056112578,24.7210824259432,0.));
#6651=CARTESIAN_POINT('Ctrl Pts',(58.1907610187597,24.2110514283266,0.));
#6652=CARTESIAN_POINT('Ctrl Pts',(58.3142240203109,23.5838111702086,0.));
#6653=CARTESIAN_POINT('Ctrl Pts',(58.4856917608691,22.9665891529976,0.));
#6654=CARTESIAN_POINT('Ctrl Pts',(58.7040649536582,22.3593331170216,0.));
#6655=CARTESIAN_POINT('Ctrl Pts',(58.9670233800433,21.7613919711372,0.));
#6656=CARTESIAN_POINT('Ctrl Pts',(59.2705528391893,21.1716763589853,0.));
#6657=CARTESIAN_POINT('Ctrl Pts',(59.6094227136446,20.5888495299376,0.));
#6658=CARTESIAN_POINT('Ctrl Pts',(59.9775897880897,20.0114964775053,0.));
#6659=CARTESIAN_POINT('Ctrl Pts',(60.3686078898803,19.4382992332324,0.));
#6660=CARTESIAN_POINT('Ctrl Pts',(60.7760056975964,18.8682016392444,0.));
#6661=CARTESIAN_POINT('Ctrl Pts',(61.1936904784186,18.3005942681782,0.));
#6662=CARTESIAN_POINT('Ctrl Pts',(61.6158386260792,17.7351881055358,0.));
#6663=CARTESIAN_POINT('Ctrl Pts',(62.0367583558289,17.1718725504246,0.));
#6664=CARTESIAN_POINT('Ctrl Pts',(62.4507485326533,16.6105738821721,0.));
#6665=CARTESIAN_POINT('Ctrl Pts',(62.8519889360609,16.0511281710465,0.));
#6666=CARTESIAN_POINT('Ctrl Pts',(63.2343441839831,15.4931095154543,0.));
#6667=CARTESIAN_POINT('Ctrl Pts',(63.5915578634715,14.9358503082954,0.));
#6668=CARTESIAN_POINT('Ctrl Pts',(63.9176667121215,14.3785717762628,0.));
#6669=CARTESIAN_POINT('Ctrl Pts',(64.2073839217625,13.8204835129561,0.));
#6670=CARTESIAN_POINT('Ctrl Pts',(64.4564605946371,13.2608853560062,0.));
#6671=CARTESIAN_POINT('Ctrl Pts',(64.6622177060836,12.6992939860082,0.));
#6672=CARTESIAN_POINT('Ctrl Pts',(64.7991653885414,12.2202610291617,0.));
#6673=CARTESIAN_POINT('Ctrl Pts',(64.8801800932063,11.8527445341239,0.));
#6674=CARTESIAN_POINT('Ctrl Pts',(64.9249249220199,11.5977782643751,0.));
#6675=CARTESIAN_POINT('Ctrl Pts',(64.9462790584754,11.4560498922985,0.));
#6676=CARTESIAN_POINT('Ctrl Pts',(64.9503835492167,11.4278882091416,0.));
#6677=CARTESIAN_POINT('Ctrl Pts',(58.1000072797208,25.4986314827289,2.38697950294409E-14));
#6678=CARTESIAN_POINT('Ctrl Pts',(58.1000072797208,25.4986314827289,3.81441588205112));
#6679=CARTESIAN_POINT('Ctrl Pts',(58.1000072797208,23.7594464132255,11.4410395120049));
#6680=CARTESIAN_POINT('Ctrl Pts',(58.1000072797208,16.4420132235113,20.6165782938419));
#6681=CARTESIAN_POINT('Ctrl Pts',(58.1000072797208,5.8680831928706,25.709427795297));
#6682=CARTESIAN_POINT('Ctrl Pts',(58.1000072797208,-4.56335585676364,25.7079717649665));
#6683=CARTESIAN_POINT('Ctrl Pts',(58.1000072797208,-12.9396099811428,22.4138494830494));
#6684=CARTESIAN_POINT('Ctrl Pts',(58.1000072797208,-18.9752754976121,17.6048416816306));
#6685=CARTESIAN_POINT('Ctrl Pts',(58.1000072797208,-23.3123262403551,11.2305682370571));
#6686=CARTESIAN_POINT('Ctrl Pts',(58.1000072797208,-26.3703094632176,1.3980365463646));
#6687=CARTESIAN_POINT('Ctrl Pts',(58.1000072797208,-24.7834831225059,-9.10809204222051));
#6688=CARTESIAN_POINT('Ctrl Pts',(58.1000072797208,-18.9691368355184,-17.602615750836));
#6689=CARTESIAN_POINT('Ctrl Pts',(58.1000072797208,-12.9426554227937,-22.4171076785279));
#6690=CARTESIAN_POINT('Ctrl Pts',(58.1000072797208,-5.76030348627288,-25.2270747172432));
#6691=CARTESIAN_POINT('Ctrl Pts',(58.1000072797208,4.50410772030096,-26.0198514690206));
#6692=CARTESIAN_POINT('Ctrl Pts',(58.1000072797208,15.6329016549998,-21.6519940090828));
#6693=CARTESIAN_POINT('Ctrl Pts',(58.1000072797208,23.7567819506992,-11.4335435336754));
#6694=CARTESIAN_POINT('Ctrl Pts',(58.1000072797208,25.4986314827281,-3.81441588205099));
#6695=CARTESIAN_POINT('Ctrl Pts',(58.1000072797208,25.4986314827281,7.66053886991358E-14));
#6696=CARTESIAN_POINT('Origin',(66.5,0.,0.));
#6697=CARTESIAN_POINT('',(67.,-1.40834381901946E-15,11.5));
#6698=CARTESIAN_POINT('Origin',(66.5,-1.40834381901946E-15,11.5));
#6699=CARTESIAN_POINT('Origin',(67.,0.,0.));
#6700=CARTESIAN_POINT('Origin',(67.,11.,0.));
#6701=CARTESIAN_POINT('',(67.,12.5828687521281,-3.88578058618805E-15));
#6702=CARTESIAN_POINT('Ctrl Pts',(67.,12.5828687521281,-4.42954684098673E-15));
#6703=CARTESIAN_POINT('Ctrl Pts',(67.,12.5828687521281,-1.88230864242211));
#6704=CARTESIAN_POINT('Ctrl Pts',(67.,11.723903698598,-5.64071163506987));
#6705=CARTESIAN_POINT('Ctrl Pts',(67.,7.71284902408557,-10.6871388545133));
#6706=CARTESIAN_POINT('Ctrl Pts',(67.,2.22487832877622,-12.8362645212214));
#6707=CARTESIAN_POINT('Ctrl Pts',(67.,-4.11571491706988,-12.3615954421279));
#6708=CARTESIAN_POINT('Ctrl Pts',(67.,-8.6464168302479,-9.7416764263013));
#6709=CARTESIAN_POINT('Ctrl Pts',(67.,-12.2290791603529,-4.48959736793348));
#6710=CARTESIAN_POINT('Ctrl Pts',(67.,-13.010200205145,0.686125352829048));
#6711=CARTESIAN_POINT('Ctrl Pts',(67.,-11.1355356277156,6.76267604165808));
#6712=CARTESIAN_POINT('Ctrl Pts',(67.,-7.57288094607568,10.6000612069797));
#6713=CARTESIAN_POINT('Ctrl Pts',(67.,-2.24885032695964,12.6844091193373));
#6714=CARTESIAN_POINT('Ctrl Pts',(67.,2.89442276640883,12.6874499975273));
#6715=CARTESIAN_POINT('Ctrl Pts',(67.,8.11457746630642,10.1730735192044));
#6716=CARTESIAN_POINT('Ctrl Pts',(67.,11.7240714096075,5.64603610965329));
#6717=CARTESIAN_POINT('Ctrl Pts',(67.,12.5828687521281,1.8823086424221));
#6718=CARTESIAN_POINT('Ctrl Pts',(67.,12.5828687521281,8.21727726654077E-16));
#6719=CARTESIAN_POINT('Ctrl Pts',(66.9987790562313,12.6177894202923,8.32667268468867E-16));
#6720=CARTESIAN_POINT('Ctrl Pts',(66.9987790562313,12.6177894202923,1.88753252870585));
#6721=CARTESIAN_POINT('Ctrl Pts',(66.9987790562313,11.7566086962385,5.66170529903387));
#6722=CARTESIAN_POINT('Ctrl Pts',(66.9987790562313,8.13709748718362,10.2013063913397));
#6723=CARTESIAN_POINT('Ctrl Pts',(66.9987790562312,2.90245552737485,12.7226609053052));
#6724=CARTESIAN_POINT('Ctrl Pts',(66.9987790562313,-2.25509145984958,12.7196115879031));
#6725=CARTESIAN_POINT('Ctrl Pts',(66.9987790562313,-7.59389762103065,10.6294790787878));
#6726=CARTESIAN_POINT('Ctrl Pts',(66.9987790562313,-11.1664395775339,6.78144419148183));
#6727=CARTESIAN_POINT('Ctrl Pts',(66.9987790562313,-13.0463068270182,0.688029525576709));
#6728=CARTESIAN_POINT('Ctrl Pts',(66.9987790562313,-12.2630179722188,-4.50205714502921));
#6729=CARTESIAN_POINT('Ctrl Pts',(66.9987790562313,-8.67041284092607,-9.76871206154051));
#6730=CARTESIAN_POINT('Ctrl Pts',(66.9987790562313,-4.12713707506171,-12.3959020204541));
#6731=CARTESIAN_POINT('Ctrl Pts',(66.9987790562313,2.23105293326073,-12.8718884272354));
#6732=CARTESIAN_POINT('Ctrl Pts',(66.9987790562313,7.73425414613492,-10.7167983889895));
#6733=CARTESIAN_POINT('Ctrl Pts',(66.9987790562313,11.7564405197882,-5.65636604767626));
#6734=CARTESIAN_POINT('Ctrl Pts',(66.9987790562313,12.6177894202922,-1.88753252870586));
#6735=CARTESIAN_POINT('Ctrl Pts',(66.9987790562313,12.6177894202922,-4.44089209850063E-15));
#6736=CARTESIAN_POINT('Ctrl Pts',(66.9995926873144,12.6061681608754,8.28565575401122E-16));
#6737=CARTESIAN_POINT('Ctrl Pts',(66.9995926873144,12.6061681608754,1.88579407027011));
#6738=CARTESIAN_POINT('Ctrl Pts',(66.9995926873144,11.7457806031927,5.65649074488443));
#6739=CARTESIAN_POINT('Ctrl Pts',(66.9995926873144,8.12960304295226,10.191910765725));
#6740=CARTESIAN_POINT('Ctrl Pts',(66.9995926873143,2.8997823025916,12.7109430570306));
#6741=CARTESIAN_POINT('Ctrl Pts',(66.9995926873144,-2.25301447135012,12.7078965482737));
#6742=CARTESIAN_POINT('Ctrl Pts',(66.9995926873143,-7.58690347578576,10.6196890965696));
#6743=CARTESIAN_POINT('Ctrl Pts',(66.9995926873144,-11.1561550431592,6.77519833358192));
#6744=CARTESIAN_POINT('Ctrl Pts',(66.9995926873144,-13.0342908938368,0.687395835367529));
#6745=CARTESIAN_POINT('Ctrl Pts',(66.9995926873144,-12.2517234652816,-4.49791065210782));
#6746=CARTESIAN_POINT('Ctrl Pts',(66.9995926873144,-8.6624272014315,-9.75971486475775));
#6747=CARTESIAN_POINT('Ctrl Pts',(66.9995926873144,-4.12333589187291,-12.3844851243478));
#6748=CARTESIAN_POINT('Ctrl Pts',(66.9995926873143,2.22899808482832,-12.8600331372316));
#6749=CARTESIAN_POINT('Ctrl Pts',(66.9995926873144,7.7271307294426,-10.7069279839104));
#6750=CARTESIAN_POINT('Ctrl Pts',(66.9995926873144,11.745612581646,-5.65115641111024));
#6751=CARTESIAN_POINT('Ctrl Pts',(66.9995926873144,12.6061681608753,-1.88579407027012));
#6752=CARTESIAN_POINT('Ctrl Pts',(66.9995926873144,12.6061681608753,-4.43755947288309E-15));
#6753=CARTESIAN_POINT('Ctrl Pts',(67.,12.5945184588186,8.24916091886633E-16));
#6754=CARTESIAN_POINT('Ctrl Pts',(67.,12.5945184588186,1.88405135674166));
#6755=CARTESIAN_POINT('Ctrl Pts',(67.,11.7349260085885,5.65126342830562));
#6756=CARTESIAN_POINT('Ctrl Pts',(67.,8.12209025615349,10.1824921443827));
#6757=CARTESIAN_POINT('Ctrl Pts',(67.,2.89710253505555,12.6991965296307));
#6758=CARTESIAN_POINT('Ctrl Pts',(67.,-2.25093239955722,12.6961528361925));
#6759=CARTESIAN_POINT('Ctrl Pts',(67.,-7.57989221236772,10.6098751537225));
#6760=CARTESIAN_POINT('Ctrl Pts',(67.,-11.1458453375251,6.76893718890919));
#6761=CARTESIAN_POINT('Ctrl Pts',(67.,-13.0222455519134,0.686760594224371));
#6762=CARTESIAN_POINT('Ctrl Pts',(67.,-12.2404013151221,-4.49375401083788));
#6763=CARTESIAN_POINT('Ctrl Pts',(67.,-8.65442201741998,-9.75069564737116));
#6764=CARTESIAN_POINT('Ctrl Pts',(67.,-4.11952540525758,-12.3730402855533));
#6765=CARTESIAN_POINT('Ctrl Pts',(67.,2.22693820721373,-12.8481488316227));
#6766=CARTESIAN_POINT('Ctrl Pts',(67.,7.71998987822122,-10.6970334212052));
#6767=CARTESIAN_POINT('Ctrl Pts',(67.,11.7347581423126,-5.64593402412958));
#6768=CARTESIAN_POINT('Ctrl Pts',(67.,12.5945184588185,-1.88405135674167));
#6769=CARTESIAN_POINT('Ctrl Pts',(67.,12.5945184588185,-4.43377464066931E-15));
#6770=CARTESIAN_POINT('Ctrl Pts',(67.,12.5828687521281,8.21727726654077E-16));
#6771=CARTESIAN_POINT('Ctrl Pts',(67.,12.5828687521281,1.8823086424221));
#6772=CARTESIAN_POINT('Ctrl Pts',(67.,11.7240714096075,5.64603610965329));
#6773=CARTESIAN_POINT('Ctrl Pts',(67.,8.11457746630642,10.1730735192044));
#6774=CARTESIAN_POINT('Ctrl Pts',(67.,2.89442276640883,12.6874499975273));
#6775=CARTESIAN_POINT('Ctrl Pts',(67.,-2.24885032695964,12.6844091193373));
#6776=CARTESIAN_POINT('Ctrl Pts',(67.,-7.57288094607568,10.6000612069797));
#6777=CARTESIAN_POINT('Ctrl Pts',(67.,-11.1355356277156,6.76267604165808));
#6778=CARTESIAN_POINT('Ctrl Pts',(67.,-13.010200205145,0.686125352829048));
#6779=CARTESIAN_POINT('Ctrl Pts',(67.,-12.2290791603529,-4.48959736793348));
#6780=CARTESIAN_POINT('Ctrl Pts',(67.,-8.6464168302479,-9.7416764263013));
#6781=CARTESIAN_POINT('Ctrl Pts',(67.,-4.11571491706988,-12.3615954421279));
#6782=CARTESIAN_POINT('Ctrl Pts',(67.,2.22487832877622,-12.8362645212214));
#6783=CARTESIAN_POINT('Ctrl Pts',(67.,7.71284902408557,-10.6871388545133));
#6784=CARTESIAN_POINT('Ctrl Pts',(67.,11.723903698598,-5.64071163506987));
#6785=CARTESIAN_POINT('Ctrl Pts',(67.,12.5828687521281,-1.88230864242211));
#6786=CARTESIAN_POINT('Ctrl Pts',(67.,12.5828687521281,-4.42954684098673E-15));
#6787=CARTESIAN_POINT('',(66.9987790562313,12.6177894202923,-2.22044604925031E-15));
#6788=CARTESIAN_POINT('Origin',(66.5,12.5828687521281,1.38777878078145E-15));
#6789=CARTESIAN_POINT('Ctrl Pts',(66.9987790562313,12.6177894202923,8.32667268468867E-16));
#6790=CARTESIAN_POINT('Ctrl Pts',(66.9987790562313,12.6177894202923,1.88753252870585));
#6791=CARTESIAN_POINT('Ctrl Pts',(66.9987790562313,11.7566086962385,5.66170529903387));
#6792=CARTESIAN_POINT('Ctrl Pts',(66.9987790562313,8.13709748718362,10.2013063913397));
#6793=CARTESIAN_POINT('Ctrl Pts',(66.9987790562312,2.90245552737485,12.7226609053052));
#6794=CARTESIAN_POINT('Ctrl Pts',(66.9987790562313,-2.25509145984958,12.7196115879031));
#6795=CARTESIAN_POINT('Ctrl Pts',(66.9987790562313,-7.59389762103065,10.6294790787878));
#6796=CARTESIAN_POINT('Ctrl Pts',(66.9987790562313,-11.1664395775339,6.78144419148183));
#6797=CARTESIAN_POINT('Ctrl Pts',(66.9987790562313,-13.0463068270182,0.688029525576709));
#6798=CARTESIAN_POINT('Ctrl Pts',(66.9987790562313,-12.2630179722188,-4.50205714502921));
#6799=CARTESIAN_POINT('Ctrl Pts',(66.9987790562313,-8.67041284092607,-9.76871206154051));
#6800=CARTESIAN_POINT('Ctrl Pts',(66.9987790562313,-4.12713707506171,-12.3959020204541));
#6801=CARTESIAN_POINT('Ctrl Pts',(66.9987790562313,2.23105293326073,-12.8718884272354));
#6802=CARTESIAN_POINT('Ctrl Pts',(66.9987790562313,7.73425414613492,-10.7167983889895));
#6803=CARTESIAN_POINT('Ctrl Pts',(66.9987790562313,11.7564405197882,-5.65636604767626));
#6804=CARTESIAN_POINT('Ctrl Pts',(66.9987790562313,12.6177894202922,-1.88753252870586));
#6805=CARTESIAN_POINT('Ctrl Pts',(66.9987790562313,12.6177894202922,-4.44089209850063E-15));
#6806=CARTESIAN_POINT('Ctrl Pts',(67.,12.6,0.));
#6807=CARTESIAN_POINT('Ctrl Pts',(67.,12.6,12.6));
#6808=CARTESIAN_POINT('Ctrl Pts',(67.,0.,12.6));
#6809=CARTESIAN_POINT('Ctrl Pts',(67.,-12.6,12.6));
#6810=CARTESIAN_POINT('Ctrl Pts',(67.,-12.6,0.));
#6811=CARTESIAN_POINT('Ctrl Pts',(67.,-12.6,-12.6));
#6812=CARTESIAN_POINT('Ctrl Pts',(67.,0.,-12.6));
#6813=CARTESIAN_POINT('Ctrl Pts',(67.,12.6,-12.6));
#6814=CARTESIAN_POINT('Ctrl Pts',(67.,12.6,0.));
#6815=CARTESIAN_POINT('Ctrl Pts',(66.9932926583693,12.6997352662803,0.));
#6816=CARTESIAN_POINT('Ctrl Pts',(66.9932926583693,12.6997352662803,12.6997352662803));
#6817=CARTESIAN_POINT('Ctrl Pts',(66.9932926583693,0.,12.6997352662803));
#6818=CARTESIAN_POINT('Ctrl Pts',(66.9932926583693,-12.6997352662803,12.6997352662803));
#6819=CARTESIAN_POINT('Ctrl Pts',(66.9932926583693,-12.6997352662803,0.));
#6820=CARTESIAN_POINT('Ctrl Pts',(66.9932926583693,-12.6997352662803,-12.6997352662803));
#6821=CARTESIAN_POINT('Ctrl Pts',(66.9932926583693,0.,-12.6997352662803));
#6822=CARTESIAN_POINT('Ctrl Pts',(66.9932926583693,12.6997352662803,-12.6997352662803));
#6823=CARTESIAN_POINT('Ctrl Pts',(66.9932926583693,12.6997352662803,0.));
#6824=CARTESIAN_POINT('Ctrl Pts',(66.9758353862889,12.9017721172185,0.));
#6825=CARTESIAN_POINT('Ctrl Pts',(66.9758353862889,12.9017721172185,12.9017721172185));
#6826=CARTESIAN_POINT('Ctrl Pts',(66.9758353862889,0.,12.9017721172185));
#6827=CARTESIAN_POINT('Ctrl Pts',(66.9758353862889,-12.9017721172185,12.9017721172185));
#6828=CARTESIAN_POINT('Ctrl Pts',(66.9758353862889,-12.9017721172185,0.));
#6829=CARTESIAN_POINT('Ctrl Pts',(66.9758353862889,-12.9017721172185,-12.9017721172185));
#6830=CARTESIAN_POINT('Ctrl Pts',(66.9758353862889,0.,-12.9017721172185));
#6831=CARTESIAN_POINT('Ctrl Pts',(66.9758353862889,12.9017721172185,-12.9017721172185));
#6832=CARTESIAN_POINT('Ctrl Pts',(66.9758353862889,12.9017721172185,0.));
#6833=CARTESIAN_POINT('Ctrl Pts',(66.9375217173852,13.2125265684525,0.));
#6834=CARTESIAN_POINT('Ctrl Pts',(66.9375217173852,13.2125265684525,13.2125265684525));
#6835=CARTESIAN_POINT('Ctrl Pts',(66.9375217173852,0.,13.2125265684525));
#6836=CARTESIAN_POINT('Ctrl Pts',(66.9375217173852,-13.2125265684525,13.2125265684525));
#6837=CARTESIAN_POINT('Ctrl Pts',(66.9375217173852,-13.2125265684525,0.));
#6838=CARTESIAN_POINT('Ctrl Pts',(66.9375217173852,-13.2125265684525,-13.2125265684525));
#6839=CARTESIAN_POINT('Ctrl Pts',(66.9375217173852,0.,-13.2125265684525));
#6840=CARTESIAN_POINT('Ctrl Pts',(66.9375217173852,13.2125265684525,-13.2125265684525));
#6841=CARTESIAN_POINT('Ctrl Pts',(66.9375217173852,13.2125265684525,0.));
#6842=CARTESIAN_POINT('Ctrl Pts',(66.8621179770906,13.6423024645368,0.));
#6843=CARTESIAN_POINT('Ctrl Pts',(66.8621179770906,13.6423024645368,13.6423024645368));
#6844=CARTESIAN_POINT('Ctrl Pts',(66.8621179770906,0.,13.6423024645368));
#6845=CARTESIAN_POINT('Ctrl Pts',(66.8621179770906,-13.6423024645368,13.6423024645368));
#6846=CARTESIAN_POINT('Ctrl Pts',(66.8621179770906,-13.6423024645368,0.));
#6847=CARTESIAN_POINT('Ctrl Pts',(66.8621179770906,-13.6423024645368,-13.6423024645368));
#6848=CARTESIAN_POINT('Ctrl Pts',(66.8621179770906,0.,-13.6423024645368));
#6849=CARTESIAN_POINT('Ctrl Pts',(66.8621179770906,13.6423024645368,-13.6423024645368));
#6850=CARTESIAN_POINT('Ctrl Pts',(66.8621179770906,13.6423024645368,0.));
#6851=CARTESIAN_POINT('Ctrl Pts',(66.7270226914732,14.2049623954268,0.));
#6852=CARTESIAN_POINT('Ctrl Pts',(66.7270226914732,14.2049623954268,14.2049623954268));
#6853=CARTESIAN_POINT('Ctrl Pts',(66.7270226914732,0.,14.2049623954268));
#6854=CARTESIAN_POINT('Ctrl Pts',(66.7270226914732,-14.2049623954268,14.2049623954268));
#6855=CARTESIAN_POINT('Ctrl Pts',(66.7270226914732,-14.2049623954268,0.));
#6856=CARTESIAN_POINT('Ctrl Pts',(66.7270226914732,-14.2049623954268,-14.2049623954268));
#6857=CARTESIAN_POINT('Ctrl Pts',(66.7270226914732,0.,-14.2049623954268));
#6858=CARTESIAN_POINT('Ctrl Pts',(66.7270226914732,14.2049623954268,-14.2049623954268));
#6859=CARTESIAN_POINT('Ctrl Pts',(66.7270226914732,14.2049623954268,0.));
#6860=CARTESIAN_POINT('Ctrl Pts',(66.5508049999324,14.7917496047061,0.));
#6861=CARTESIAN_POINT('Ctrl Pts',(66.5508049999324,14.7917496047061,14.7917496047061));
#6862=CARTESIAN_POINT('Ctrl Pts',(66.5508049999324,0.,14.7917496047061));
#6863=CARTESIAN_POINT('Ctrl Pts',(66.5508049999324,-14.7917496047061,14.7917496047061));
#6864=CARTESIAN_POINT('Ctrl Pts',(66.5508049999324,-14.7917496047061,0.));
#6865=CARTESIAN_POINT('Ctrl Pts',(66.5508049999324,-14.7917496047061,-14.7917496047061));
#6866=CARTESIAN_POINT('Ctrl Pts',(66.5508049999324,0.,-14.7917496047061));
#6867=CARTESIAN_POINT('Ctrl Pts',(66.5508049999324,14.7917496047061,-14.7917496047061));
#6868=CARTESIAN_POINT('Ctrl Pts',(66.5508049999324,14.7917496047061,0.));
#6869=CARTESIAN_POINT('Ctrl Pts',(66.333400353284,15.3997739599779,0.));
#6870=CARTESIAN_POINT('Ctrl Pts',(66.333400353284,15.3997739599778,15.3997739599778));
#6871=CARTESIAN_POINT('Ctrl Pts',(66.333400353284,0.,15.3997739599779));
#6872=CARTESIAN_POINT('Ctrl Pts',(66.333400353284,-15.3997739599778,15.3997739599778));
#6873=CARTESIAN_POINT('Ctrl Pts',(66.333400353284,-15.3997739599779,0.));
#6874=CARTESIAN_POINT('Ctrl Pts',(66.333400353284,-15.3997739599778,-15.3997739599778));
#6875=CARTESIAN_POINT('Ctrl Pts',(66.333400353284,0.,-15.3997739599779));
#6876=CARTESIAN_POINT('Ctrl Pts',(66.333400353284,15.3997739599778,-15.3997739599778));
#6877=CARTESIAN_POINT('Ctrl Pts',(66.333400353284,15.3997739599779,0.));
#6878=CARTESIAN_POINT('Ctrl Pts',(66.0751703194864,16.0237534171383,0.));
#6879=CARTESIAN_POINT('Ctrl Pts',(66.0751703194864,16.0237534171383,16.0237534171383));
#6880=CARTESIAN_POINT('Ctrl Pts',(66.0751703194864,0.,16.0237534171383));
#6881=CARTESIAN_POINT('Ctrl Pts',(66.0751703194864,-16.0237534171383,16.0237534171383));
#6882=CARTESIAN_POINT('Ctrl Pts',(66.0751703194864,-16.0237534171383,0.));
#6883=CARTESIAN_POINT('Ctrl Pts',(66.0751703194864,-16.0237534171383,-16.0237534171383));
#6884=CARTESIAN_POINT('Ctrl Pts',(66.0751703194864,0.,-16.0237534171383));
#6885=CARTESIAN_POINT('Ctrl Pts',(66.0751703194864,16.0237534171383,-16.0237534171383));
#6886=CARTESIAN_POINT('Ctrl Pts',(66.0751703194864,16.0237534171383,0.));
#6887=CARTESIAN_POINT('Ctrl Pts',(65.7771152465929,16.6559365250315,0.));
#6888=CARTESIAN_POINT('Ctrl Pts',(65.7771152465929,16.6559365250315,16.6559365250315));
#6889=CARTESIAN_POINT('Ctrl Pts',(65.7771152465929,0.,16.6559365250315));
#6890=CARTESIAN_POINT('Ctrl Pts',(65.7771152465929,-16.6559365250315,16.6559365250315));
#6891=CARTESIAN_POINT('Ctrl Pts',(65.7771152465929,-16.6559365250315,0.));
#6892=CARTESIAN_POINT('Ctrl Pts',(65.7771152465929,-16.6559365250315,-16.6559365250315));
#6893=CARTESIAN_POINT('Ctrl Pts',(65.7771152465929,0.,-16.6559365250315));
#6894=CARTESIAN_POINT('Ctrl Pts',(65.7771152465929,16.6559365250315,-16.6559365250315));
#6895=CARTESIAN_POINT('Ctrl Pts',(65.7771152465929,16.6559365250315,0.));
#6896=CARTESIAN_POINT('Ctrl Pts',(65.4410849670182,17.2875976116165,0.));
#6897=CARTESIAN_POINT('Ctrl Pts',(65.4410849670182,17.2875976116165,17.2875976116165));
#6898=CARTESIAN_POINT('Ctrl Pts',(65.4410849670182,0.,17.2875976116165));
#6899=CARTESIAN_POINT('Ctrl Pts',(65.4410849670182,-17.2875976116165,17.2875976116165));
#6900=CARTESIAN_POINT('Ctrl Pts',(65.4410849670182,-17.2875976116165,0.));
#6901=CARTESIAN_POINT('Ctrl Pts',(65.4410849670182,-17.2875976116165,-17.2875976116165));
#6902=CARTESIAN_POINT('Ctrl Pts',(65.4410849670182,0.,-17.2875976116165));
#6903=CARTESIAN_POINT('Ctrl Pts',(65.4410849670182,17.2875976116165,-17.2875976116165));
#6904=CARTESIAN_POINT('Ctrl Pts',(65.4410849670182,17.2875976116165,0.));
#6905=CARTESIAN_POINT('Ctrl Pts',(65.0700058995025,17.9101691052111,0.));
#6906=CARTESIAN_POINT('Ctrl Pts',(65.0700058995025,17.9101691052111,17.9101691052111));
#6907=CARTESIAN_POINT('Ctrl Pts',(65.0700058995025,0.,17.9101691052111));
#6908=CARTESIAN_POINT('Ctrl Pts',(65.0700058995025,-17.9101691052111,17.9101691052111));
#6909=CARTESIAN_POINT('Ctrl Pts',(65.0700058995025,-17.9101691052111,0.));
#6910=CARTESIAN_POINT('Ctrl Pts',(65.0700058995025,-17.9101691052111,-17.9101691052111));
#6911=CARTESIAN_POINT('Ctrl Pts',(65.0700058995025,0.,-17.9101691052111));
#6912=CARTESIAN_POINT('Ctrl Pts',(65.0700058995025,17.9101691052111,-17.9101691052111));
#6913=CARTESIAN_POINT('Ctrl Pts',(65.0700058995025,17.9101691052111,0.));
#6914=CARTESIAN_POINT('Ctrl Pts',(64.6681449587856,18.5165543814796,0.));
#6915=CARTESIAN_POINT('Ctrl Pts',(64.6681449587856,18.5165543814796,18.5165543814796));
#6916=CARTESIAN_POINT('Ctrl Pts',(64.6681449587856,0.,18.5165543814796));
#6917=CARTESIAN_POINT('Ctrl Pts',(64.6681449587856,-18.5165543814796,18.5165543814796));
#6918=CARTESIAN_POINT('Ctrl Pts',(64.6681449587856,-18.5165543814796,0.));
#6919=CARTESIAN_POINT('Ctrl Pts',(64.6681449587856,-18.5165543814796,-18.5165543814796));
#6920=CARTESIAN_POINT('Ctrl Pts',(64.6681449587856,0.,-18.5165543814796));
#6921=CARTESIAN_POINT('Ctrl Pts',(64.6681449587856,18.5165543814796,-18.5165543814796));
#6922=CARTESIAN_POINT('Ctrl Pts',(64.6681449587856,18.5165543814796,0.));
#6923=CARTESIAN_POINT('Ctrl Pts',(64.241353075389,19.1022896867918,0.));
#6924=CARTESIAN_POINT('Ctrl Pts',(64.241353075389,19.1022896867918,19.1022896867918));
#6925=CARTESIAN_POINT('Ctrl Pts',(64.241353075389,0.,19.1022896867918));
#6926=CARTESIAN_POINT('Ctrl Pts',(64.241353075389,-19.1022896867918,19.1022896867918));
#6927=CARTESIAN_POINT('Ctrl Pts',(64.241353075389,-19.1022896867918,0.));
#6928=CARTESIAN_POINT('Ctrl Pts',(64.241353075389,-19.1022896867918,-19.1022896867918));
#6929=CARTESIAN_POINT('Ctrl Pts',(64.241353075389,0.,-19.1022896867918));
#6930=CARTESIAN_POINT('Ctrl Pts',(64.241353075389,19.1022896867918,-19.1022896867918));
#6931=CARTESIAN_POINT('Ctrl Pts',(64.241353075389,19.1022896867918,0.));
#6932=CARTESIAN_POINT('Ctrl Pts',(63.7974413872401,19.6670367803137,0.));
#6933=CARTESIAN_POINT('Ctrl Pts',(63.7974413872401,19.6670367803137,19.6670367803137));
#6934=CARTESIAN_POINT('Ctrl Pts',(63.7974413872401,0.,19.6670367803137));
#6935=CARTESIAN_POINT('Ctrl Pts',(63.7974413872401,-19.6670367803137,19.6670367803137));
#6936=CARTESIAN_POINT('Ctrl Pts',(63.7974413872401,-19.6670367803137,0.));
#6937=CARTESIAN_POINT('Ctrl Pts',(63.7974413872401,-19.6670367803137,-19.6670367803137));
#6938=CARTESIAN_POINT('Ctrl Pts',(63.7974413872401,0.,-19.6670367803137));
#6939=CARTESIAN_POINT('Ctrl Pts',(63.7974413872401,19.6670367803137,-19.6670367803137));
#6940=CARTESIAN_POINT('Ctrl Pts',(63.7974413872401,19.6670367803137,0.));
#6941=CARTESIAN_POINT('Ctrl Pts',(63.345612386475,20.2136468221279,0.));
#6942=CARTESIAN_POINT('Ctrl Pts',(63.345612386475,20.2136468221279,20.2136468221279));
#6943=CARTESIAN_POINT('Ctrl Pts',(63.345612386475,0.,20.2136468221279));
#6944=CARTESIAN_POINT('Ctrl Pts',(63.345612386475,-20.2136468221279,20.2136468221279));
#6945=CARTESIAN_POINT('Ctrl Pts',(63.345612386475,-20.2136468221279,0.));
#6946=CARTESIAN_POINT('Ctrl Pts',(63.345612386475,-20.2136468221279,-20.2136468221279));
#6947=CARTESIAN_POINT('Ctrl Pts',(63.345612386475,0.,-20.2136468221279));
#6948=CARTESIAN_POINT('Ctrl Pts',(63.345612386475,20.2136468221279,-20.2136468221279));
#6949=CARTESIAN_POINT('Ctrl Pts',(63.345612386475,20.2136468221279,0.));
#6950=CARTESIAN_POINT('Ctrl Pts',(62.8957596029255,20.7468804921309,0.));
#6951=CARTESIAN_POINT('Ctrl Pts',(62.8957596029255,20.7468804921309,20.7468804921309));
#6952=CARTESIAN_POINT('Ctrl Pts',(62.8957596029255,0.,20.7468804921309));
#6953=CARTESIAN_POINT('Ctrl Pts',(62.8957596029255,-20.7468804921309,20.7468804921309));
#6954=CARTESIAN_POINT('Ctrl Pts',(62.8957596029255,-20.7468804921309,0.));
#6955=CARTESIAN_POINT('Ctrl Pts',(62.8957596029255,-20.7468804921309,-20.7468804921309));
#6956=CARTESIAN_POINT('Ctrl Pts',(62.8957596029255,0.,-20.7468804921309));
#6957=CARTESIAN_POINT('Ctrl Pts',(62.8957596029255,20.7468804921309,-20.7468804921309));
#6958=CARTESIAN_POINT('Ctrl Pts',(62.8957596029255,20.7468804921309,0.));
#6959=CARTESIAN_POINT('Ctrl Pts',(62.4578085440914,21.2722425632023,0.));
#6960=CARTESIAN_POINT('Ctrl Pts',(62.4578085440914,21.2722425632023,21.2722425632023));
#6961=CARTESIAN_POINT('Ctrl Pts',(62.4578085440914,0.,21.2722425632023));
#6962=CARTESIAN_POINT('Ctrl Pts',(62.4578085440914,-21.2722425632023,21.2722425632023));
#6963=CARTESIAN_POINT('Ctrl Pts',(62.4578085440914,-21.2722425632023,0.));
#6964=CARTESIAN_POINT('Ctrl Pts',(62.4578085440914,-21.2722425632023,-21.2722425632023));
#6965=CARTESIAN_POINT('Ctrl Pts',(62.4578085440914,0.,-21.2722425632023));
#6966=CARTESIAN_POINT('Ctrl Pts',(62.4578085440914,21.2722425632023,-21.2722425632023));
#6967=CARTESIAN_POINT('Ctrl Pts',(62.4578085440914,21.2722425632023,0.));
#6968=CARTESIAN_POINT('Ctrl Pts',(62.0410846718656,21.7948710346798,0.));
#6969=CARTESIAN_POINT('Ctrl Pts',(62.0410846718656,21.7948710346798,21.7948710346798));
#6970=CARTESIAN_POINT('Ctrl Pts',(62.0410846718656,0.,21.7948710346798));
#6971=CARTESIAN_POINT('Ctrl Pts',(62.0410846718656,-21.7948710346798,21.7948710346798));
#6972=CARTESIAN_POINT('Ctrl Pts',(62.0410846718656,-21.7948710346798,0.));
#6973=CARTESIAN_POINT('Ctrl Pts',(62.0410846718656,-21.7948710346798,-21.7948710346798));
#6974=CARTESIAN_POINT('Ctrl Pts',(62.0410846718656,0.,-21.7948710346798));
#6975=CARTESIAN_POINT('Ctrl Pts',(62.0410846718656,21.7948710346798,-21.7948710346798));
#6976=CARTESIAN_POINT('Ctrl Pts',(62.0410846718656,21.7948710346798,0.));
#6977=CARTESIAN_POINT('Ctrl Pts',(61.6535606725113,22.3182034793593,0.));
#6978=CARTESIAN_POINT('Ctrl Pts',(61.6535606725113,22.3182034793593,22.3182034793593));
#6979=CARTESIAN_POINT('Ctrl Pts',(61.6535606725113,0.,22.3182034793593));
#6980=CARTESIAN_POINT('Ctrl Pts',(61.6535606725113,-22.3182034793593,22.3182034793593));
#6981=CARTESIAN_POINT('Ctrl Pts',(61.6535606725113,-22.3182034793593,0.));
#6982=CARTESIAN_POINT('Ctrl Pts',(61.6535606725113,-22.3182034793593,-22.3182034793593));
#6983=CARTESIAN_POINT('Ctrl Pts',(61.6535606725113,0.,-22.3182034793593));
#6984=CARTESIAN_POINT('Ctrl Pts',(61.6535606725113,22.3182034793593,-22.3182034793593));
#6985=CARTESIAN_POINT('Ctrl Pts',(61.6535606725113,22.3182034793593,0.));
#6986=CARTESIAN_POINT('Ctrl Pts',(61.3014818178065,22.8434269247565,0.));
#6987=CARTESIAN_POINT('Ctrl Pts',(61.3014818178065,22.8434269247565,22.8434269247565));
#6988=CARTESIAN_POINT('Ctrl Pts',(61.3014818178065,0.,22.8434269247565));
#6989=CARTESIAN_POINT('Ctrl Pts',(61.3014818178065,-22.8434269247565,22.8434269247565));
#6990=CARTESIAN_POINT('Ctrl Pts',(61.3014818178065,-22.8434269247565,0.));
#6991=CARTESIAN_POINT('Ctrl Pts',(61.3014818178065,-22.8434269247565,-22.8434269247565));
#6992=CARTESIAN_POINT('Ctrl Pts',(61.3014818178065,0.,-22.8434269247565));
#6993=CARTESIAN_POINT('Ctrl Pts',(61.3014818178065,22.8434269247565,-22.8434269247565));
#6994=CARTESIAN_POINT('Ctrl Pts',(61.3014818178065,22.8434269247565,0.));
#6995=CARTESIAN_POINT('Ctrl Pts',(60.9896656117218,23.370292675902,0.));
#6996=CARTESIAN_POINT('Ctrl Pts',(60.9896656117218,23.370292675902,23.370292675902));
#6997=CARTESIAN_POINT('Ctrl Pts',(60.9896656117218,0.,23.370292675902));
#6998=CARTESIAN_POINT('Ctrl Pts',(60.9896656117218,-23.370292675902,23.370292675902));
#6999=CARTESIAN_POINT('Ctrl Pts',(60.9896656117218,-23.370292675902,0.));
#7000=CARTESIAN_POINT('Ctrl Pts',(60.9896656117218,-23.370292675902,-23.370292675902));
#7001=CARTESIAN_POINT('Ctrl Pts',(60.9896656117218,0.,-23.370292675902));
#7002=CARTESIAN_POINT('Ctrl Pts',(60.9896656117218,23.370292675902,-23.370292675902));
#7003=CARTESIAN_POINT('Ctrl Pts',(60.9896656117218,23.370292675902,0.));
#7004=CARTESIAN_POINT('Ctrl Pts',(60.7216146343454,23.8976229480199,0.));
#7005=CARTESIAN_POINT('Ctrl Pts',(60.7216146343454,23.8976229480199,23.8976229480199));
#7006=CARTESIAN_POINT('Ctrl Pts',(60.7216146343454,0.,23.8976229480199));
#7007=CARTESIAN_POINT('Ctrl Pts',(60.7216146343454,-23.8976229480199,23.8976229480199));
#7008=CARTESIAN_POINT('Ctrl Pts',(60.7216146343454,-23.8976229480199,0.));
#7009=CARTESIAN_POINT('Ctrl Pts',(60.7216146343454,-23.8976229480199,-23.8976229480199));
#7010=CARTESIAN_POINT('Ctrl Pts',(60.7216146343454,0.,-23.8976229480199));
#7011=CARTESIAN_POINT('Ctrl Pts',(60.7216146343454,23.8976229480199,-23.8976229480199));
#7012=CARTESIAN_POINT('Ctrl Pts',(60.7216146343454,23.8976229480199,0.));
#7013=CARTESIAN_POINT('Ctrl Pts',(60.4996857760211,24.4238918300188,0.));
#7014=CARTESIAN_POINT('Ctrl Pts',(60.4996857760211,24.4238918300188,24.4238918300188));
#7015=CARTESIAN_POINT('Ctrl Pts',(60.4996857760211,0.,24.4238918300188));
#7016=CARTESIAN_POINT('Ctrl Pts',(60.4996857760211,-24.4238918300188,24.4238918300188));
#7017=CARTESIAN_POINT('Ctrl Pts',(60.4996857760211,-24.4238918300188,0.));
#7018=CARTESIAN_POINT('Ctrl Pts',(60.4996857760211,-24.4238918300188,-24.4238918300188));
#7019=CARTESIAN_POINT('Ctrl Pts',(60.4996857760211,0.,-24.4238918300188));
#7020=CARTESIAN_POINT('Ctrl Pts',(60.4996857760211,24.4238918300188,-24.4238918300188));
#7021=CARTESIAN_POINT('Ctrl Pts',(60.4996857760211,24.4238918300188,0.));
#7022=CARTESIAN_POINT('Ctrl Pts',(60.3251702155445,24.947858058,0.));
#7023=CARTESIAN_POINT('Ctrl Pts',(60.3251702155445,24.947858058,24.947858058));
#7024=CARTESIAN_POINT('Ctrl Pts',(60.3251702155445,0.,24.947858058));
#7025=CARTESIAN_POINT('Ctrl Pts',(60.3251702155445,-24.947858058,24.947858058));
#7026=CARTESIAN_POINT('Ctrl Pts',(60.3251702155445,-24.947858058,0.));
#7027=CARTESIAN_POINT('Ctrl Pts',(60.3251702155445,-24.947858058,-24.947858058));
#7028=CARTESIAN_POINT('Ctrl Pts',(60.3251702155445,0.,-24.947858058));
#7029=CARTESIAN_POINT('Ctrl Pts',(60.3251702155445,24.947858058,-24.947858058));
#7030=CARTESIAN_POINT('Ctrl Pts',(60.3251702155445,24.947858058,0.));
#7031=CARTESIAN_POINT('Ctrl Pts',(60.1984961951092,25.4688514249257,0.));
#7032=CARTESIAN_POINT('Ctrl Pts',(60.1984961951092,25.4688514249257,25.4688514249257));
#7033=CARTESIAN_POINT('Ctrl Pts',(60.1984961951092,0.,25.4688514249257));
#7034=CARTESIAN_POINT('Ctrl Pts',(60.1984961951092,-25.4688514249257,25.4688514249257));
#7035=CARTESIAN_POINT('Ctrl Pts',(60.1984961951092,-25.4688514249257,0.));
#7036=CARTESIAN_POINT('Ctrl Pts',(60.1984961951092,-25.4688514249257,-25.4688514249257));
#7037=CARTESIAN_POINT('Ctrl Pts',(60.1984961951092,0.,-25.4688514249257));
#7038=CARTESIAN_POINT('Ctrl Pts',(60.1984961951092,25.4688514249257,-25.4688514249257));
#7039=CARTESIAN_POINT('Ctrl Pts',(60.1984961951092,25.4688514249257,0.));
#7040=CARTESIAN_POINT('Ctrl Pts',(60.1353708288129,25.8830038831508,0.));
#7041=CARTESIAN_POINT('Ctrl Pts',(60.1353708288129,25.8830038831508,25.8830038831508));
#7042=CARTESIAN_POINT('Ctrl Pts',(60.1353708288129,0.,25.8830038831508));
#7043=CARTESIAN_POINT('Ctrl Pts',(60.1353708288129,-25.8830038831508,25.8830038831508));
#7044=CARTESIAN_POINT('Ctrl Pts',(60.1353708288129,-25.8830038831508,0.));
#7045=CARTESIAN_POINT('Ctrl Pts',(60.1353708288129,-25.8830038831508,-25.8830038831508));
#7046=CARTESIAN_POINT('Ctrl Pts',(60.1353708288129,0.,-25.8830038831508));
#7047=CARTESIAN_POINT('Ctrl Pts',(60.1353708288129,25.8830038831508,-25.8830038831508));
#7048=CARTESIAN_POINT('Ctrl Pts',(60.1353708288129,25.8830038831508,0.));
#7049=CARTESIAN_POINT('Ctrl Pts',(60.1093965237418,26.1920935983768,0.));
#7050=CARTESIAN_POINT('Ctrl Pts',(60.1093965237418,26.1920935983768,26.1920935983768));
#7051=CARTESIAN_POINT('Ctrl Pts',(60.1093965237418,0.,26.1920935983768));
#7052=CARTESIAN_POINT('Ctrl Pts',(60.1093965237418,-26.1920935983768,26.1920935983768));
#7053=CARTESIAN_POINT('Ctrl Pts',(60.1093965237418,-26.1920935983768,0.));
#7054=CARTESIAN_POINT('Ctrl Pts',(60.1093965237418,-26.1920935983768,-26.1920935983768));
#7055=CARTESIAN_POINT('Ctrl Pts',(60.1093965237418,0.,-26.1920935983768));
#7056=CARTESIAN_POINT('Ctrl Pts',(60.1093965237418,26.1920935983768,-26.1920935983768));
#7057=CARTESIAN_POINT('Ctrl Pts',(60.1093965237418,26.1920935983768,0.));
#7058=CARTESIAN_POINT('Ctrl Pts',(60.1015533409406,26.3974772180319,0.));
#7059=CARTESIAN_POINT('Ctrl Pts',(60.1015533409406,26.3974772180319,26.3974772180319));
#7060=CARTESIAN_POINT('Ctrl Pts',(60.1015533409406,0.,26.3974772180319));
#7061=CARTESIAN_POINT('Ctrl Pts',(60.1015533409406,-26.3974772180319,26.3974772180319));
#7062=CARTESIAN_POINT('Ctrl Pts',(60.1015533409406,-26.3974772180319,0.));
#7063=CARTESIAN_POINT('Ctrl Pts',(60.1015533409406,-26.3974772180319,-26.3974772180319));
#7064=CARTESIAN_POINT('Ctrl Pts',(60.1015533409406,0.,-26.3974772180319));
#7065=CARTESIAN_POINT('Ctrl Pts',(60.1015533409406,26.3974772180319,-26.3974772180319));
#7066=CARTESIAN_POINT('Ctrl Pts',(60.1015533409406,26.3974772180319,0.));
#7067=CARTESIAN_POINT('Ctrl Pts',(60.1,26.5,0.));
#7068=CARTESIAN_POINT('Ctrl Pts',(60.1,26.5,26.5));
#7069=CARTESIAN_POINT('Ctrl Pts',(60.1,0.,26.5));
#7070=CARTESIAN_POINT('Ctrl Pts',(60.1,-26.5,26.5));
#7071=CARTESIAN_POINT('Ctrl Pts',(60.1,-26.5,0.));
#7072=CARTESIAN_POINT('Ctrl Pts',(60.1,-26.5,-26.5));
#7073=CARTESIAN_POINT('Ctrl Pts',(60.1,0.,-26.5));
#7074=CARTESIAN_POINT('Ctrl Pts',(60.1,26.5,-26.5));
#7075=CARTESIAN_POINT('Ctrl Pts',(60.1,26.5,0.));
#7076=CARTESIAN_POINT('',(60.1000630537694,26.4959364690653,9.43689570931383E-15));
#7077=CARTESIAN_POINT('Ctrl Pts',(66.9987790562313,12.6177894202923,0.));
#7078=CARTESIAN_POINT('Ctrl Pts',(66.9920328774672,12.714146473408,0.));
#7079=CARTESIAN_POINT('Ctrl Pts',(66.9744621413525,12.9128524924851,0.));
#7080=CARTESIAN_POINT('Ctrl Pts',(66.9361754064266,13.2201869184335,0.));
#7081=CARTESIAN_POINT('Ctrl Pts',(66.8611550018322,13.6463131714231,0.));
#7082=CARTESIAN_POINT('Ctrl Pts',(66.7270226914732,14.2049623954268,0.));
#7083=CARTESIAN_POINT('Ctrl Pts',(66.5508049999324,14.7917496047061,0.));
#7084=CARTESIAN_POINT('Ctrl Pts',(66.333400353284,15.3997739599779,0.));
#7085=CARTESIAN_POINT('Ctrl Pts',(66.0751703194864,16.0237534171383,0.));
#7086=CARTESIAN_POINT('Ctrl Pts',(65.7771152465929,16.6559365250315,0.));
#7087=CARTESIAN_POINT('Ctrl Pts',(65.4410849670182,17.2875976116165,0.));
#7088=CARTESIAN_POINT('Ctrl Pts',(65.0700058995025,17.9101691052111,0.));
#7089=CARTESIAN_POINT('Ctrl Pts',(64.6681449587856,18.5165543814796,0.));
#7090=CARTESIAN_POINT('Ctrl Pts',(64.241353075389,19.1022896867918,0.));
#7091=CARTESIAN_POINT('Ctrl Pts',(63.7974413872401,19.6670367803137,0.));
#7092=CARTESIAN_POINT('Ctrl Pts',(63.345612386475,20.2136468221279,0.));
#7093=CARTESIAN_POINT('Ctrl Pts',(62.8957596029255,20.7468804921309,0.));
#7094=CARTESIAN_POINT('Ctrl Pts',(62.4578085440914,21.2722425632023,0.));
#7095=CARTESIAN_POINT('Ctrl Pts',(62.0410846718656,21.7948710346798,0.));
#7096=CARTESIAN_POINT('Ctrl Pts',(61.6535606725113,22.3182034793593,0.));
#7097=CARTESIAN_POINT('Ctrl Pts',(61.3014818178065,22.8434269247565,0.));
#7098=CARTESIAN_POINT('Ctrl Pts',(60.9896656117218,23.370292675902,0.));
#7099=CARTESIAN_POINT('Ctrl Pts',(60.7216146343454,23.8976229480199,0.));
#7100=CARTESIAN_POINT('Ctrl Pts',(60.4996857760211,24.4238918300188,0.));
#7101=CARTESIAN_POINT('Ctrl Pts',(60.3251702155445,24.947858058,0.));
#7102=CARTESIAN_POINT('Ctrl Pts',(60.1986970208453,25.4680254554329,0.));
#7103=CARTESIAN_POINT('Ctrl Pts',(60.1356211722196,25.8813624061185,0.));
#7104=CARTESIAN_POINT('Ctrl Pts',(60.1096028663132,26.1896434519942,0.));
#7105=CARTESIAN_POINT('Ctrl Pts',(60.101678577611,26.3942210551826,0.));
#7106=CARTESIAN_POINT('Ctrl Pts',(60.1000630537672,26.4959364692063,0.));
#7107=CARTESIAN_POINT('Ctrl Pts',(60.1000630537694,26.4959364690656,1.88737914186277E-14));
#7108=CARTESIAN_POINT('Ctrl Pts',(60.1000630537694,26.4959364690656,-3.9636056917746));
#7109=CARTESIAN_POINT('Ctrl Pts',(60.1000630537694,24.685961262727,-11.8807347957342));
#7110=CARTESIAN_POINT('Ctrl Pts',(60.1000630537695,16.2443369841089,-22.4988484266417));
#7111=CARTESIAN_POINT('Ctrl Pts',(60.1000630537694,4.68027293296291,-27.0375433673444));
#7112=CARTESIAN_POINT('Ctrl Pts',(60.1000630537694,-5.98560140555878,-26.2137571448923));
#7113=CARTESIAN_POINT('Ctrl Pts',(60.1000630537694,-13.4488703508335,-23.2938884734323));
#7114=CARTESIAN_POINT('Ctrl Pts',(60.1000630537694,-19.7110570984953,-18.2910903026092));
#7115=CARTESIAN_POINT('Ctrl Pts',(60.1000630537694,-25.752819385365,-9.46432907623452));
#7116=CARTESIAN_POINT('Ctrl Pts',(60.1000630537694,-27.4017087341173,1.45271682099757));
#7117=CARTESIAN_POINT('Ctrl Pts',(60.1000630537694,-24.2241191010755,11.6698194289465));
#7118=CARTESIAN_POINT('Ctrl Pts',(60.1000630537694,-19.717439049817,18.2934039326558));
#7119=CARTESIAN_POINT('Ctrl Pts',(60.1000630537694,-13.4457047614966,23.2905009850213));
#7120=CARTESIAN_POINT('Ctrl Pts',(60.1000630537694,-4.74183848087839,26.7134634764109));
#7121=CARTESIAN_POINT('Ctrl Pts',(60.1000630537694,6.09759643163882,26.714979249407));
#7122=CARTESIAN_POINT('Ctrl Pts',(60.1000630537694,17.0850948456638,21.4229364239694));
#7123=CARTESIAN_POINT('Ctrl Pts',(60.1000630537694,24.6887294488487,11.8885228778762));
#7124=CARTESIAN_POINT('Ctrl Pts',(60.1000630537694,26.4959364690658,3.9636056917746));
#7125=CARTESIAN_POINT('Ctrl Pts',(60.1000630537694,26.4959364690658,-1.72084568816899E-14));
#7126=CARTESIAN_POINT('Ctrl Pts',(60.1000630537694,26.4959364690658,-1.72084568816899E-14));
#7127=CARTESIAN_POINT('Ctrl Pts',(60.1000630537694,26.4959364690658,3.9636056917746));
#7128=CARTESIAN_POINT('Ctrl Pts',(60.1000630537694,24.6887294488487,11.8885228778762));
#7129=CARTESIAN_POINT('Ctrl Pts',(60.1000630537694,17.0850948456638,21.4229364239694));
#7130=CARTESIAN_POINT('Ctrl Pts',(60.1000630537694,6.09759643163882,26.714979249407));
#7131=CARTESIAN_POINT('Ctrl Pts',(60.1000630537694,-4.74183848087839,26.7134634764109));
#7132=CARTESIAN_POINT('Ctrl Pts',(60.1000630537694,-13.4457047614966,23.2905009850213));
#7133=CARTESIAN_POINT('Ctrl Pts',(60.1000630537694,-19.717439049817,18.2934039326558));
#7134=CARTESIAN_POINT('Ctrl Pts',(60.1000630537694,-24.2241191010755,11.6698194289465));
#7135=CARTESIAN_POINT('Ctrl Pts',(60.1000630537694,-27.4017087341173,1.45271682099757));
#7136=CARTESIAN_POINT('Ctrl Pts',(60.1000630537694,-25.752819385365,-9.46432907623452));
#7137=CARTESIAN_POINT('Ctrl Pts',(60.1000630537694,-19.7110570984953,-18.2910903026092));
#7138=CARTESIAN_POINT('Ctrl Pts',(60.1000630537694,-13.4488703508335,-23.2938884734323));
#7139=CARTESIAN_POINT('Ctrl Pts',(60.1000630537694,-5.98560140555878,-26.2137571448923));
#7140=CARTESIAN_POINT('Ctrl Pts',(60.1000630537694,4.68027293296291,-27.0375433673444));
#7141=CARTESIAN_POINT('Ctrl Pts',(60.1000630537695,16.2443369841089,-22.4988484266417));
#7142=CARTESIAN_POINT('Ctrl Pts',(60.1000630537694,24.685961262727,-11.8807347957342));
#7143=CARTESIAN_POINT('Ctrl Pts',(60.1000630537694,26.4959364690656,-3.9636056917746));
#7144=CARTESIAN_POINT('Ctrl Pts',(60.1000630537694,26.4959364690656,1.88737914186277E-14));
#7145=CARTESIAN_POINT('Ctrl Pts',(60.1000210188067,26.4985830432097,-1.72080134116452E-14));
#7146=CARTESIAN_POINT('Ctrl Pts',(60.1000210188067,26.4985830432097,3.96400160064724));
#7147=CARTESIAN_POINT('Ctrl Pts',(60.1000210188067,24.6911955082417,11.8897103753363));
#7148=CARTESIAN_POINT('Ctrl Pts',(60.1000210188067,17.0868014081141,21.4250762762329));
#7149=CARTESIAN_POINT('Ctrl Pts',(60.1000210188067,6.09820549639387,26.7176477028667));
#7150=CARTESIAN_POINT('Ctrl Pts',(60.1000210188066,-4.74231212434193,26.716131778466));
#7151=CARTESIAN_POINT('Ctrl Pts',(60.1000210188067,-13.4470477996871,23.2928273809114));
#7152=CARTESIAN_POINT('Ctrl Pts',(60.1000210188066,-19.7194085467032,18.2952311883147));
#7153=CARTESIAN_POINT('Ctrl Pts',(60.1000210188067,-24.2265387523811,11.6709850809853));
#7154=CARTESIAN_POINT('Ctrl Pts',(60.1000210188066,-27.404445782265,1.45286192712664));
#7155=CARTESIAN_POINT('Ctrl Pts',(60.1000210188067,-25.7553917324869,-9.46527443057792));
#7156=CARTESIAN_POINT('Ctrl Pts',(60.1000210188066,-19.7130259579137,-18.2929173271688));
#7157=CARTESIAN_POINT('Ctrl Pts',(60.1000210188067,-13.4502137052222,-23.2962152076852));
#7158=CARTESIAN_POINT('Ctrl Pts',(60.1000210188067,-5.98619928357432,-26.2163755332612));
#7159=CARTESIAN_POINT('Ctrl Pts',(60.1000210188067,4.6807404268877,-27.0402440404561));
#7160=CARTESIAN_POINT('Ctrl Pts',(60.1000210188067,16.2459595665867,-22.5010957474934));
#7161=CARTESIAN_POINT('Ctrl Pts',(60.1000210188067,24.6884270456168,-11.8819215152736));
#7162=CARTESIAN_POINT('Ctrl Pts',(60.1000210188067,26.4985830432095,-3.96400160064724));
#7163=CARTESIAN_POINT('Ctrl Pts',(60.1000210188067,26.4985830432095,1.88736805511165E-14));
#7164=CARTESIAN_POINT('Ctrl Pts',(60.1,26.5012299511459,-1.72076166127272E-14));
#7165=CARTESIAN_POINT('Ctrl Pts',(60.1,26.5012299511459,3.96439755945304));
#7166=CARTESIAN_POINT('Ctrl Pts',(60.1,24.6936618786601,11.8908980225664));
#7167=CARTESIAN_POINT('Ctrl Pts',(60.1,17.0885081858003,21.4272163983797));
#7168=CARTESIAN_POINT('Ctrl Pts',(60.1,6.09881463796566,26.720316492878));
#7169=CARTESIAN_POINT('Ctrl Pts',(60.1,-4.74278582754248,26.7188004170537));
#7170=CARTESIAN_POINT('Ctrl Pts',(60.1,-13.4483910072647,23.2951540702122));
#7171=CARTESIAN_POINT('Ctrl Pts',(60.1,-19.7213782919872,18.2970586744316));
#7172=CARTESIAN_POINT('Ctrl Pts',(60.1,-24.2289587088591,11.6721508800389));
#7173=CARTESIAN_POINT('Ctrl Pts',(60.1,-27.4071831756158,1.45300705155683));
#7174=CARTESIAN_POINT('Ctrl Pts',(60.1,-25.7579644040394,-9.46621990415165));
#7175=CARTESIAN_POINT('Ctrl Pts',(60.1,-19.7149950656494,-18.2947445821571));
#7176=CARTESIAN_POINT('Ctrl Pts',(60.1,-13.4515572290378,-23.2985422353914));
#7177=CARTESIAN_POINT('Ctrl Pts',(60.1,-5.98679723699566,-26.2189942518676));
#7178=CARTESIAN_POINT('Ctrl Pts',(60.1,4.68120797977395,-27.0429450541832));
#7179=CARTESIAN_POINT('Ctrl Pts',(60.1,16.2475823537085,-22.5033433517827));
#7180=CARTESIAN_POINT('Ctrl Pts',(60.1,24.6908931394971,-11.8831083844848));
#7181=CARTESIAN_POINT('Ctrl Pts',(60.1,26.5012299511458,-3.96439755945305));
#7182=CARTESIAN_POINT('Ctrl Pts',(60.1,26.5012299511458,1.88735230124792E-14));
#7183=CARTESIAN_POINT('Ctrl Pts',(60.1,26.503876859085,-1.72072665349743E-14));
#7184=CARTESIAN_POINT('Ctrl Pts',(60.1,26.503876859085,3.9647935182593));
#7185=CARTESIAN_POINT('Ctrl Pts',(60.1,24.6961282490811,11.8920856697977));
#7186=CARTESIAN_POINT('Ctrl Pts',(60.1,17.0902149634882,21.4293565205288));
#7187=CARTESIAN_POINT('Ctrl Pts',(60.1,6.09942377953813,26.7229852828923));
#7188=CARTESIAN_POINT('Ctrl Pts',(60.1,-4.74325953074353,26.7214690556444));
#7189=CARTESIAN_POINT('Ctrl Pts',(60.1,-13.4497342148437,23.2974807595154));
#7190=CARTESIAN_POINT('Ctrl Pts',(60.1,-19.7233480372732,18.2988861605503));
#7191=CARTESIAN_POINT('Ctrl Pts',(60.1,-24.2313786653396,11.6733166790938));
#7192=CARTESIAN_POINT('Ctrl Pts',(60.1,-27.4099205689696,1.45315217598718));
#7193=CARTESIAN_POINT('Ctrl Pts',(60.1,-25.7605370755947,-9.46716537772638));
#7194=CARTESIAN_POINT('Ctrl Pts',(60.1,-19.7169641733872,-18.2965718371474));
#7195=CARTESIAN_POINT('Ctrl Pts',(60.1,-13.4529007528549,-23.3008692631002));
#7196=CARTESIAN_POINT('Ctrl Pts',(60.1,-5.98739519041764,-26.2216129704768));
#7197=CARTESIAN_POINT('Ctrl Pts',(60.1,4.68167553266069,-27.0456460679132));
#7198=CARTESIAN_POINT('Ctrl Pts',(60.1,16.249205140832,-22.5055909560744));
#7199=CARTESIAN_POINT('Ctrl Pts',(60.1,24.6933592333801,-11.8842952536973));
#7200=CARTESIAN_POINT('Ctrl Pts',(60.1,26.5038768590848,-3.9647935182593));
#7201=CARTESIAN_POINT('Ctrl Pts',(60.1,26.5038768590848,1.88733188225822E-14));
#7202=CARTESIAN_POINT('',(60.1,26.503876859085,-1.83186799063151E-14));
#7203=CARTESIAN_POINT('Origin',(60.6,26.503876859085,-1.83186799063151E-14));
#7204=CARTESIAN_POINT('Ctrl Pts',(60.1,26.503876859085,-1.72072665349743E-14));
#7205=CARTESIAN_POINT('Ctrl Pts',(60.1,26.503876859085,3.9647935182593));
#7206=CARTESIAN_POINT('Ctrl Pts',(60.1,24.6961282490811,11.8920856697977));
#7207=CARTESIAN_POINT('Ctrl Pts',(60.1,17.0902149634882,21.4293565205288));
#7208=CARTESIAN_POINT('Ctrl Pts',(60.1,6.09942377953813,26.7229852828923));
#7209=CARTESIAN_POINT('Ctrl Pts',(60.1,-4.74325953074353,26.7214690556444));
#7210=CARTESIAN_POINT('Ctrl Pts',(60.1,-13.4497342148437,23.2974807595154));
#7211=CARTESIAN_POINT('Ctrl Pts',(60.1,-19.7233480372732,18.2988861605503));
#7212=CARTESIAN_POINT('Ctrl Pts',(60.1,-24.2313786653396,11.6733166790938));
#7213=CARTESIAN_POINT('Ctrl Pts',(60.1,-27.4099205689696,1.45315217598718));
#7214=CARTESIAN_POINT('Ctrl Pts',(60.1,-25.7605370755947,-9.46716537772638));
#7215=CARTESIAN_POINT('Ctrl Pts',(60.1,-19.7169641733872,-18.2965718371474));
#7216=CARTESIAN_POINT('Ctrl Pts',(60.1,-13.4529007528549,-23.3008692631002));
#7217=CARTESIAN_POINT('Ctrl Pts',(60.1,-5.98739519041764,-26.2216129704768));
#7218=CARTESIAN_POINT('Ctrl Pts',(60.1,4.68167553266069,-27.0456460679132));
#7219=CARTESIAN_POINT('Ctrl Pts',(60.1,16.249205140832,-22.5055909560744));
#7220=CARTESIAN_POINT('Ctrl Pts',(60.1,24.6933592333801,-11.8842952536973));
#7221=CARTESIAN_POINT('Ctrl Pts',(60.1,26.5038768590848,-3.9647935182593));
#7222=CARTESIAN_POINT('Ctrl Pts',(60.1,26.5038768590848,1.88733188225822E-14));
#7223=CARTESIAN_POINT('Origin',(60.1,26.5,0.));
#7224=CARTESIAN_POINT('',(60.1,57.4230311248647,-2.97413793103448));
#7225=CARTESIAN_POINT('',(60.1,57.4230311248647,2.97413793103448));
#7226=CARTESIAN_POINT('Origin',(60.1,0.,0.));
#7227=CARTESIAN_POINT('Origin',(60.1,0.,0.));
#7228=CARTESIAN_POINT('Ctrl Pts',(58.1000072797208,25.4986314827289,2.38697950294409E-14));
#7229=CARTESIAN_POINT('Ctrl Pts',(58.1000072797208,25.4986314827289,3.81441588205112));
#7230=CARTESIAN_POINT('Ctrl Pts',(58.1000072797208,23.7594464132255,11.4410395120049));
#7231=CARTESIAN_POINT('Ctrl Pts',(58.1000072797208,16.4420132235113,20.6165782938419));
#7232=CARTESIAN_POINT('Ctrl Pts',(58.1000072797208,5.8680831928706,25.709427795297));
#7233=CARTESIAN_POINT('Ctrl Pts',(58.1000072797208,-4.56335585676364,25.7079717649665));
#7234=CARTESIAN_POINT('Ctrl Pts',(58.1000072797208,-12.9396099811428,22.4138494830494));
#7235=CARTESIAN_POINT('Ctrl Pts',(58.1000072797208,-18.9752754976121,17.6048416816306));
#7236=CARTESIAN_POINT('Ctrl Pts',(58.1000072797208,-23.3123262403551,11.2305682370571));
#7237=CARTESIAN_POINT('Ctrl Pts',(58.1000072797208,-26.3703094632176,1.3980365463646));
#7238=CARTESIAN_POINT('Ctrl Pts',(58.1000072797208,-24.7834831225059,-9.10809204222051));
#7239=CARTESIAN_POINT('Ctrl Pts',(58.1000072797208,-18.9691368355184,-17.602615750836));
#7240=CARTESIAN_POINT('Ctrl Pts',(58.1000072797208,-12.9426554227937,-22.4171076785279));
#7241=CARTESIAN_POINT('Ctrl Pts',(58.1000072797208,-5.76030348627288,-25.2270747172432));
#7242=CARTESIAN_POINT('Ctrl Pts',(58.1000072797208,4.50410772030096,-26.0198514690206));
#7243=CARTESIAN_POINT('Ctrl Pts',(58.1000072797208,15.6329016549998,-21.6519940090828));
#7244=CARTESIAN_POINT('Ctrl Pts',(58.1000072797208,23.7567819506992,-11.4335435336754));
#7245=CARTESIAN_POINT('Ctrl Pts',(58.1000072797208,25.4986314827281,-3.81441588205099));
#7246=CARTESIAN_POINT('Ctrl Pts',(58.1000072797208,25.4986314827281,7.66053886991358E-14));
#7247=CARTESIAN_POINT('Ctrl Pts',(58.1000024265854,25.4995308359835,2.3870421523717E-14));
#7248=CARTESIAN_POINT('Ctrl Pts',(58.1000024265854,25.4995308359835,3.81455041897088));
#7249=CARTESIAN_POINT('Ctrl Pts',(58.1000024265854,23.7602844242958,11.4414430448819));
#7250=CARTESIAN_POINT('Ctrl Pts',(58.1000024265854,16.4425931439715,20.6173054539171));
#7251=CARTESIAN_POINT('Ctrl Pts',(58.1000024265854,5.86829016396711,25.7103345834742));
#7252=CARTESIAN_POINT('Ctrl Pts',(58.1000024265854,-4.56351680928159,25.7088785017885));
#7253=CARTESIAN_POINT('Ctrl Pts',(58.1000024265854,-12.9400663695712,22.4146400340441));
#7254=CARTESIAN_POINT('Ctrl Pts',(58.1000024265854,-18.9759447678742,17.605462615804));
#7255=CARTESIAN_POINT('Ctrl Pts',(58.1000024265854,-23.3131484812071,11.2309643464758));
#7256=CARTESIAN_POINT('Ctrl Pts',(58.1000024265854,-26.3712395611192,1.39808585601947));
#7257=CARTESIAN_POINT('Ctrl Pts',(58.1000024265854,-24.7843572520144,-9.10841329052855));
#7258=CARTESIAN_POINT('Ctrl Pts',(58.1000024265854,-18.9698058892659,-17.6032366064994));
#7259=CARTESIAN_POINT('Ctrl Pts',(58.1000024265854,-12.9431119186369,-22.4178983444412));
#7260=CARTESIAN_POINT('Ctrl Pts',(58.1000024265853,-5.76050665590931,-25.2279644925147));
#7261=CARTESIAN_POINT('Ctrl Pts',(58.1000024265854,4.50426658309875,-26.0207692060419));
#7262=CARTESIAN_POINT('Ctrl Pts',(58.1000024265854,15.6334530375707,-21.6527576889412));
#7263=CARTESIAN_POINT('Ctrl Pts',(58.1000024265854,23.7576198677921,-11.4339468021644));
#7264=CARTESIAN_POINT('Ctrl Pts',(58.1000024265854,25.4995308359827,-3.81455041897075));
#7265=CARTESIAN_POINT('Ctrl Pts',(58.1000024265854,25.4995308359827,7.66056040565432E-14));
#7266=CARTESIAN_POINT('Ctrl Pts',(58.1,25.5004302023323,2.38710372417893E-14));
#7267=CARTESIAN_POINT('Ctrl Pts',(58.1,25.5004302023323,3.81468495784946));
#7268=CARTESIAN_POINT('Ctrl Pts',(58.1,23.7611224475672,11.4418465836341));
#7269=CARTESIAN_POINT('Ctrl Pts',(58.1,16.4431730728752,20.6180326245795));
#7270=CARTESIAN_POINT('Ctrl Pts',(58.1,5.86849713807706,25.7112413848538));
#7271=CARTESIAN_POINT('Ctrl Pts',(58.1,-4.56367776414296,25.7097852518122));
#7272=CARTESIAN_POINT('Ctrl Pts',(58.1,-12.9405227646445,22.4154305965488));
#7273=CARTESIAN_POINT('Ctrl Pts',(58.1,-18.9766140478806,17.606083559018));
#7274=CARTESIAN_POINT('Ctrl Pts',(58.1,-23.3139707340307,11.2313604616617));
#7275=CARTESIAN_POINT('Ctrl Pts',(58.1000000000001,-26.3721696725628,1.39813516639225));
#7276=CARTESIAN_POINT('Ctrl Pts',(58.1,-24.78523139425,-9.10873454351383));
#7277=CARTESIAN_POINT('Ctrl Pts',(58.1000000000001,-18.9704749527546,-17.6038574712023));
#7278=CARTESIAN_POINT('Ctrl Pts',(58.1,-12.9435684211264,-22.4186890218663));
#7279=CARTESIAN_POINT('Ctrl Pts',(58.1,-5.7607098285038,-25.228854280741));
#7280=CARTESIAN_POINT('Ctrl Pts',(58.1,4.50442544820952,-26.021686956425));
#7281=CARTESIAN_POINT('Ctrl Pts',(58.1,15.6340044281696,-21.6535213799185));
#7282=CARTESIAN_POINT('Ctrl Pts',(58.1,23.7584577970848,-11.4343500765248));
#7283=CARTESIAN_POINT('Ctrl Pts',(58.1,25.5004302023316,-3.81468495784933));
#7284=CARTESIAN_POINT('Ctrl Pts',(58.1,25.5004302023316,7.6605795167492E-14));
#7285=CARTESIAN_POINT('Ctrl Pts',(58.1,25.5013295686812,2.38716421746933E-14));
#7286=CARTESIAN_POINT('Ctrl Pts',(58.1,25.5013295686812,3.81481949672803));
#7287=CARTESIAN_POINT('Ctrl Pts',(58.1,23.7619604708386,11.4422501223864));
#7288=CARTESIAN_POINT('Ctrl Pts',(58.1,16.4437530017789,20.6187597952419));
#7289=CARTESIAN_POINT('Ctrl Pts',(58.1,5.86870411218699,25.7121481862334));
#7290=CARTESIAN_POINT('Ctrl Pts',(58.1,-4.56383871900433,25.7106920018359));
#7291=CARTESIAN_POINT('Ctrl Pts',(58.1,-12.9409791597178,22.4162211590536));
#7292=CARTESIAN_POINT('Ctrl Pts',(58.1,-18.977283327887,17.606704502232));
#7293=CARTESIAN_POINT('Ctrl Pts',(58.1,-23.3147929868542,11.2317565768476));
#7294=CARTESIAN_POINT('Ctrl Pts',(58.1000000000001,-26.3730997840064,1.39818447676506));
#7295=CARTESIAN_POINT('Ctrl Pts',(58.1,-24.7861055364855,-9.10905579649912));
#7296=CARTESIAN_POINT('Ctrl Pts',(58.1000000000001,-18.9711440162433,-17.6044783359051));
#7297=CARTESIAN_POINT('Ctrl Pts',(58.1,-12.944024923616,-22.4194796992914));
#7298=CARTESIAN_POINT('Ctrl Pts',(58.1,-5.76091300109831,-25.2297440689673));
#7299=CARTESIAN_POINT('Ctrl Pts',(58.1,4.5045843133203,-26.0226047068082));
#7300=CARTESIAN_POINT('Ctrl Pts',(58.1,15.6345558187685,-21.6542850708958));
#7301=CARTESIAN_POINT('Ctrl Pts',(58.1,23.7592957263775,-11.4347533508852));
#7302=CARTESIAN_POINT('Ctrl Pts',(58.1,25.5013295686804,-3.8148194967279));
#7303=CARTESIAN_POINT('Ctrl Pts',(58.1,25.5013295686804,7.66059620291998E-14));
#7304=CARTESIAN_POINT('',(58.1,25.5013295686804,7.16093850883226E-14));
#7305=CARTESIAN_POINT('Origin',(58.6,25.5013295686812,2.16493489801906E-14));
#7306=CARTESIAN_POINT('Ctrl Pts',(58.1,25.5013295686797,7.54957705575713E-14));
#7307=CARTESIAN_POINT('Ctrl Pts',(58.1,25.5013295686797,-3.81481949672779));
#7308=CARTESIAN_POINT('Ctrl Pts',(58.1,24.6303126475283,-7.62478642380632));
#7309=CARTESIAN_POINT('Ctrl Pts',(58.1,22.9760932008113,-11.0626996453471));
#7310=CARTESIAN_POINT('Ctrl Pts',(58.1,21.3218737540942,-14.500612866888));
#7311=CARTESIAN_POINT('Ctrl Pts',(58.1,18.8844517818116,-17.5664723828911));
#7312=CARTESIAN_POINT('Ctrl Pts',(58.1,15.9016432968718,-19.9424377685946));
#7313=CARTESIAN_POINT('Ctrl Pts',(58.1,11.9245653169521,-23.1103916161994));
#7314=CARTESIAN_POINT('Ctrl Pts',(58.1,6.97791131453084,-25.0518670099382));
#7315=CARTESIAN_POINT('Ctrl Pts',(58.1,1.90719420891763,-25.4347385952375));
#7316=CARTESIAN_POINT('Ctrl Pts',(58.1,-0.628164343888988,-25.6261743878872));
#7317=CARTESIAN_POINT('Ctrl Pts',(58.1,-3.19453867249359,-25.427959228427));
#7318=CARTESIAN_POINT('Ctrl Pts',(58.1,-5.67491115721548,-24.8604742537509));
#7319=CARTESIAN_POINT('Ctrl Pts',(58.1,-8.15528364193736,-24.2929892790749));
#7320=CARTESIAN_POINT('Ctrl Pts',(58.1,-10.5496542827765,-23.3562344891829));
#7321=CARTESIAN_POINT('Ctrl Pts',(58.1,-12.7513594519673,-22.0853568670059));
#7322=CARTESIAN_POINT('Ctrl Pts',(58.1,-14.9530646211581,-20.8144792448289));
#7323=CARTESIAN_POINT('Ctrl Pts',(58.1,-16.9621043187005,-19.2094787903669));
#7324=CARTESIAN_POINT('Ctrl Pts',(58.1,-18.693494357502,-17.3450507457101));
#7325=CARTESIAN_POINT('Ctrl Pts',(58.1,-20.4248843963035,-15.4806227010533));
#7326=CARTESIAN_POINT('Ctrl Pts',(58.1,-21.878624776364,-13.3567670662019));
#7327=CARTESIAN_POINT('Ctrl Pts',(58.1,-22.9800345503645,-11.0652599535289));
#7328=CARTESIAN_POINT('Ctrl Pts',(58.1,-25.1828540983653,-6.48224572818298));
#7329=CARTESIAN_POINT('Ctrl Pts',(58.1,-25.9763512221258,-1.22862559155098));
#7330=CARTESIAN_POINT('Ctrl Pts',(58.1,-25.2214146643286,3.80043848735385));
#7331=CARTESIAN_POINT('Ctrl Pts',(58.1,-24.84394638543,6.31497052680626));
#7332=CARTESIAN_POINT('Ctrl Pts',(58.1,-24.0793696861419,8.77336355182689));
#7333=CARTESIAN_POINT('Ctrl Pts',(58.1,-22.9741630600034,11.0650513852346));
#7334=CARTESIAN_POINT('Ctrl Pts',(58.1,-21.8689564338649,13.3567392186423));
#7335=CARTESIAN_POINT('Ctrl Pts',(58.1,-20.4231198808759,15.481721860437));
#7336=CARTESIAN_POINT('Ctrl Pts',(58.1,-18.6941509096865,17.3457992908047));
#7337=CARTESIAN_POINT('Ctrl Pts',(58.1,-16.9651819384971,19.2098767211723));
#7338=CARTESIAN_POINT('Ctrl Pts',(58.1,-14.9530805491074,20.8130489401129));
#7339=CARTESIAN_POINT('Ctrl Pts',(58.1,-12.7502955057392,22.0852737414092));
#7340=CARTESIAN_POINT('Ctrl Pts',(58.1,-10.547510462371,23.3574985427055));
#7341=CARTESIAN_POINT('Ctrl Pts',(58.1,-8.15404176502431,24.2987759263576));
#7342=CARTESIAN_POINT('Ctrl Pts',(58.1,-5.67470626349718,24.8636879749886));
#7343=CARTESIAN_POINT('Ctrl Pts',(58.1,-1.95570301120648,25.7110560479351));
#7344=CARTESIAN_POINT('Ctrl Pts',(58.1,1.95650055049023,25.7116021170842));
#7345=CARTESIAN_POINT('Ctrl Pts',(58.1,5.6751104796039,24.8629770864935));
#7346=CARTESIAN_POINT('Ctrl Pts',(58.1,9.39372040871756,24.0143520559028));
#7347=CARTESIAN_POINT('Ctrl Pts',(58.1,12.9187367052482,22.3165559255723));
#7348=CARTESIAN_POINT('Ctrl Pts',(58.1,15.9009460983568,19.9382395815978));
#7349=CARTESIAN_POINT('Ctrl Pts',(58.1,18.8831554914654,17.5599232376234));
#7350=CARTESIAN_POINT('Ctrl Pts',(58.1,21.322557981152,14.5010866800049));
#7351=CARTESIAN_POINT('Ctrl Pts',(58.1,22.9771015004559,11.0648107447811));
#7352=CARTESIAN_POINT('Ctrl Pts',(58.1,24.6316450197599,7.62853480955721));
#7353=CARTESIAN_POINT('Ctrl Pts',(58.1,25.5013295686812,3.81481949672803));
#7354=CARTESIAN_POINT('Ctrl Pts',(58.1,25.5013295686812,2.38716421746933E-14));
#7355=CARTESIAN_POINT('Origin',(58.1,60.5,0.));
#7356=CARTESIAN_POINT('',(58.1,-7.3111413909097E-15,59.7));
#7357=CARTESIAN_POINT('Origin',(58.1,0.,0.));
#7358=CARTESIAN_POINT('Origin',(60.55,59.9249530663145,-3.));
#7359=CARTESIAN_POINT('',(60.6,59.9478721217627,-2.50052555931523));
#7360=CARTESIAN_POINT('',(60.6,59.9249530663145,-2.5));
#7361=CARTESIAN_POINT('Origin',(60.6,59.9249530663145,-3.));
#7362=CARTESIAN_POINT('',(62.4,59.9249530663145,-2.5));
#7363=CARTESIAN_POINT('',(60.55,59.9249530663145,-2.5));
#7364=CARTESIAN_POINT('',(62.4,60.4243276752005,-3.025));
#7365=CARTESIAN_POINT('Origin',(62.4,59.9249530663145,-3.));
#7366=CARTESIAN_POINT('',(60.1,60.4243276752005,-3.025));
#7367=CARTESIAN_POINT('',(60.55,60.4243276752005,-3.025));
#7368=CARTESIAN_POINT('Ctrl Pts',(60.6,59.9478721217627,-2.50052555931523));
#7369=CARTESIAN_POINT('Ctrl Pts',(60.6,59.9513712471188,-2.50068612138112));
#7370=CARTESIAN_POINT('Ctrl Pts',(60.5999631921872,59.9548737120599,-2.50088368385959));
#7371=CARTESIAN_POINT('Ctrl Pts',(60.5988534347359,60.0074936809125,-2.50440931235234));
#7372=CARTESIAN_POINT('Ctrl Pts',(60.5905898947881,60.0547893216016,-2.51485483908352));
#7373=CARTESIAN_POINT('Ctrl Pts',(60.5587918082573,60.1527949769169,-2.55124410360599));
#7374=CARTESIAN_POINT('Ctrl Pts',(60.5329987364422,60.2000785105811,-2.57930326175212));
#7375=CARTESIAN_POINT('Ctrl Pts',(60.4622024183735,60.292853998527,-2.65468544195021));
#7376=CARTESIAN_POINT('Ctrl Pts',(60.4115325491484,60.3362328533458,-2.70762122730265));
#7377=CARTESIAN_POINT('Ctrl Pts',(60.2769563903468,60.4089098807044,-2.8463207295033));
#7378=CARTESIAN_POINT('Ctrl Pts',(60.190541226799,60.428444844956,-2.93417456909241));
#7379=CARTESIAN_POINT('Ctrl Pts',(60.1015881345704,60.4244055071003,-3.02340716123007));
#7380=CARTESIAN_POINT('Ctrl Pts',(60.1007940667366,60.4243675436247,-3.02420362885069));
#7381=CARTESIAN_POINT('Ctrl Pts',(60.1,60.4243276752005,-3.025));
#7382=CARTESIAN_POINT('Ctrl Pts',(62.4,59.9249530663145,-2.5));
#7383=CARTESIAN_POINT('Ctrl Pts',(62.4261954145561,59.9249530663145,-2.5));
#7384=CARTESIAN_POINT('Ctrl Pts',(62.4783266322709,59.9031781113224,-2.5));
#7385=CARTESIAN_POINT('Ctrl Pts',(62.5,59.8510230365392,-2.5));
#7386=CARTESIAN_POINT('Ctrl Pts',(62.5,59.8248276219832,-2.5));
#7387=CARTESIAN_POINT('Ctrl Pts',(62.4,60.0600211649479,-2.5));
#7388=CARTESIAN_POINT('Ctrl Pts',(62.4616961972161,60.0600211649479,-2.5));
#7389=CARTESIAN_POINT('Ctrl Pts',(62.5841180518885,60.0076626751897,-2.49996163393935));
#7390=CARTESIAN_POINT('Ctrl Pts',(62.6320023421471,59.8852898118316,-2.49996440018845));
#7391=CARTESIAN_POINT('Ctrl Pts',(62.6308996938996,59.8248276219832,-2.5));
#7392=CARTESIAN_POINT('Ctrl Pts',(62.4,60.3287554028045,-2.61590736409158));
#7393=CARTESIAN_POINT('Ctrl Pts',(62.5319883255722,60.3287554028045,-2.61590736409158));
#7394=CARTESIAN_POINT('Ctrl Pts',(62.7941599982643,60.2152911717712,-2.61426659004369));
#7395=CARTESIAN_POINT('Ctrl Pts',(62.8947191636549,59.9532224176658,-2.61040576784208));
#7396=CARTESIAN_POINT('Ctrl Pts',(62.8915104141356,59.8248276219832,-2.60848958586446));
#7397=CARTESIAN_POINT('Ctrl Pts',(62.4,60.4310810801322,-2.89010084214397));
#7398=CARTESIAN_POINT('Ctrl Pts',(62.5592604005367,60.4310810801322,-2.89010084214397));
#7399=CARTESIAN_POINT('Ctrl Pts',(62.8753088977623,60.2975536797591,-2.8854985007134));
#7400=CARTESIAN_POINT('Ctrl Pts',(63.0017539553834,59.9819463835178,-2.87456299295786));
#7401=CARTESIAN_POINT('Ctrl Pts',(63.,59.8248276219832,-2.86910030610043));
#7402=CARTESIAN_POINT('Ctrl Pts',(62.4,60.4243276752005,-3.02500000000001));
#7403=CARTESIAN_POINT('Ctrl Pts',(62.5571724873364,60.4243276752005,-3.02500000000001));
#7404=CARTESIAN_POINT('Ctrl Pts',(62.8699597936253,60.2939494729186,-3.01957486519097));
#7405=CARTESIAN_POINT('Ctrl Pts',(63.,59.9816715724272,-3.00655155431689));
#7406=CARTESIAN_POINT('Ctrl Pts',(63.,59.8248276219832,-3.));
#7407=CARTESIAN_POINT('',(62.5,59.8248276219832,-2.5));
#7408=CARTESIAN_POINT('',(63.,59.8248276219832,-3.));
#7409=CARTESIAN_POINT('Origin',(62.5,59.8248276219832,-3.));
#7410=CARTESIAN_POINT('Ctrl Pts',(63.,59.8248276219832,-3.));
#7411=CARTESIAN_POINT('Ctrl Pts',(63.,59.9816715724272,-3.00655155431689));
#7412=CARTESIAN_POINT('Ctrl Pts',(62.8699597936253,60.2939494729186,-3.01957486519097));
#7413=CARTESIAN_POINT('Ctrl Pts',(62.5571724873364,60.4243276752005,-3.02500000000001));
#7414=CARTESIAN_POINT('Ctrl Pts',(62.4,60.4243276752005,-3.02500000000001));
#7415=CARTESIAN_POINT('Ctrl Pts',(62.4,59.9249530663145,-2.5));
#7416=CARTESIAN_POINT('Ctrl Pts',(62.4261954145561,59.9249530663145,-2.5));
#7417=CARTESIAN_POINT('Ctrl Pts',(62.4783266322709,59.9031781113224,-2.5));
#7418=CARTESIAN_POINT('Ctrl Pts',(62.5,59.8510230365392,-2.5));
#7419=CARTESIAN_POINT('Ctrl Pts',(62.5,59.8248276219832,-2.5));
#7420=CARTESIAN_POINT('Origin',(62.5,58.25,-3.));
#7421=CARTESIAN_POINT('',(62.5,58.0224956374681,-2.5));
#7422=CARTESIAN_POINT('',(63.,58.0224956374681,-3.));
#7423=CARTESIAN_POINT('Origin',(62.5,58.0224956374681,-3.));
#7424=CARTESIAN_POINT('',(63.,58.25,-3.));
#7425=CARTESIAN_POINT('',(62.5,58.25,-2.5));
#7426=CARTESIAN_POINT('Ctrl Pts',(62.5,58.0224956374681,-2.5));
#7427=CARTESIAN_POINT('Ctrl Pts',(62.5,57.9962991377946,-2.5));
#7428=CARTESIAN_POINT('Ctrl Pts',(62.478326631158,57.9441387853006,-2.5));
#7429=CARTESIAN_POINT('Ctrl Pts',(62.4261964996734,57.9223618302983,-2.5));
#7430=CARTESIAN_POINT('Ctrl Pts',(62.4,57.9223618302983,-2.5));
#7431=CARTESIAN_POINT('Ctrl Pts',(62.6308996938996,58.0224956374681,-2.5));
#7432=CARTESIAN_POINT('Ctrl Pts',(62.6297629272861,57.9620363652066,-2.50003670134814));
#7433=CARTESIAN_POINT('Ctrl Pts',(62.5778246198969,57.8438878491714,-2.50003956584365));
#7434=CARTESIAN_POINT('Ctrl Pts',(62.4594554053708,57.795774405517,-2.5));
#7435=CARTESIAN_POINT('Ctrl Pts',(62.4,57.795774405517,-2.5));
#7436=CARTESIAN_POINT('Ctrl Pts',(62.8915113750724,58.022495637468,-2.60848862492762));
#7437=CARTESIAN_POINT('Ctrl Pts',(62.8882033397738,57.8941116945847,-2.60651315205814));
#7438=CARTESIAN_POINT('Ctrl Pts',(62.7758463976871,57.6445251096574,-2.60266612956143));
#7439=CARTESIAN_POINT('Ctrl Pts',(62.5254658026268,57.5435955938278,-2.60110845458278));
#7440=CARTESIAN_POINT('Ctrl Pts',(62.4,57.5435955938278,-2.60110845458278));
#7441=CARTESIAN_POINT('Ctrl Pts',(63.,58.0224956374681,-2.86910030610043));
#7442=CARTESIAN_POINT('Ctrl Pts',(62.998191773373,57.865391083981,-2.86346859167697));
#7443=CARTESIAN_POINT('Ctrl Pts',(62.8652984129375,57.5564336213585,-2.85232926567146));
#7444=CARTESIAN_POINT('Ctrl Pts',(62.5556992082037,57.4295787502844,-2.84771995480427));
#7445=CARTESIAN_POINT('Ctrl Pts',(62.4,57.4295787502844,-2.84771995480427));
#7446=CARTESIAN_POINT('Ctrl Pts',(63.,58.0224956374681,-3.00000000000001));
#7447=CARTESIAN_POINT('Ctrl Pts',(63.,57.8656658629709,-2.99324572615905));
#7448=CARTESIAN_POINT('Ctrl Pts',(62.8699597869483,57.5534008162154,-2.97977498708946));
#7449=CARTESIAN_POINT('Ctrl Pts',(62.5571789980404,57.4230311248647,-2.97413793103448));
#7450=CARTESIAN_POINT('Ctrl Pts',(62.4,57.4230311248647,-2.97413793103448));
#7451=CARTESIAN_POINT('',(62.4,57.9223618302983,-2.5));
#7452=CARTESIAN_POINT('',(62.4,57.4230311248647,-2.97413793103448));
#7453=CARTESIAN_POINT('Origin',(62.4,57.9223618302983,-3.));
#7454=CARTESIAN_POINT('Ctrl Pts',(62.4,57.4230311248647,-2.97413793103448));
#7455=CARTESIAN_POINT('Ctrl Pts',(62.5571789980404,57.4230311248647,-2.97413793103448));
#7456=CARTESIAN_POINT('Ctrl Pts',(62.8699597869483,57.5534008162154,-2.97977498708946));
#7457=CARTESIAN_POINT('Ctrl Pts',(63.,57.8656658629709,-2.99324572615905));
#7458=CARTESIAN_POINT('Ctrl Pts',(63.,58.0224956374681,-3.00000000000001));
#7459=CARTESIAN_POINT('Ctrl Pts',(62.5,58.0224956374681,-2.5));
#7460=CARTESIAN_POINT('Ctrl Pts',(62.5,57.9962991377946,-2.5));
#7461=CARTESIAN_POINT('Ctrl Pts',(62.478326631158,57.9441387853006,-2.5));
#7462=CARTESIAN_POINT('Ctrl Pts',(62.4261964996734,57.9223618302983,-2.5));
#7463=CARTESIAN_POINT('Ctrl Pts',(62.4,57.9223618302983,-2.5));
#7464=CARTESIAN_POINT('Origin',(61.55,57.9223618302983,-3.));
#7465=CARTESIAN_POINT('',(60.5994374367416,57.9223618302896,-2.5));
#7466=CARTESIAN_POINT('Ctrl Pts',(60.1,57.4230311248647,-2.97413793103448));
#7467=CARTESIAN_POINT('Ctrl Pts',(60.1008135540983,57.4230730234755,-2.97332897553566));
#7468=CARTESIAN_POINT('Ctrl Pts',(60.1016271094375,57.4231168880088,-2.97252012062025));
#7469=CARTESIAN_POINT('Ctrl Pts',(60.1591133854327,57.4263552929666,-2.91537316521117));
#7470=CARTESIAN_POINT('Ctrl Pts',(60.2161905779351,57.439110580143,-2.8591262187641));
#7471=CARTESIAN_POINT('Ctrl Pts',(60.3268065827896,57.4846962962046,-2.75111321481816));
#7472=CARTESIAN_POINT('Ctrl Pts',(60.3812501918161,57.5182917420481,-2.69848124864027));
#7473=CARTESIAN_POINT('Ctrl Pts',(60.4681999917132,57.5985821334825,-2.61563853552119));
#7474=CARTESIAN_POINT('Ctrl Pts',(60.5033113035832,57.6412749470976,-2.58265302130672));
#7475=CARTESIAN_POINT('Ctrl Pts',(60.554272023061,57.7307439456096,-2.53604375043298));
#7476=CARTESIAN_POINT('Ctrl Pts',(60.5724543137632,57.7744341680491,-2.51995587221209));
#7477=CARTESIAN_POINT('Ctrl Pts',(60.5927186872872,57.8544686959718,-2.50350008622553));
#7478=CARTESIAN_POINT('Ctrl Pts',(60.5978171938089,57.8882030869101,-2.5000000000006));
#7479=CARTESIAN_POINT('Ctrl Pts',(60.599437436742,57.9223618302896,-2.5));
#7480=CARTESIAN_POINT('',(61.55,57.4230311248647,-2.97413793103448));
#7481=CARTESIAN_POINT('',(61.55,57.9223618302983,-2.5));
#7482=CARTESIAN_POINT('Origin',(62.3,59.,-2.5));
#7483=CARTESIAN_POINT('',(60.6,57.9460956406901,-2.5));
#7484=CARTESIAN_POINT('',(60.6,61.5,-2.5));
#7485=CARTESIAN_POINT('Ctrl Pts',(60.6,57.9460956406901,-2.5));
#7486=CARTESIAN_POINT('Ctrl Pts',(60.6,57.9383411366579,-2.5));
#7487=CARTESIAN_POINT('Ctrl Pts',(60.5998192566414,57.9304115416576,-2.5));
#7488=CARTESIAN_POINT('Ctrl Pts',(60.599437436742,57.9223618302896,-2.5));
#7489=CARTESIAN_POINT('Origin',(61.55,57.9223618302983,3.));
#7490=CARTESIAN_POINT('',(60.5994374367416,57.9223618302896,2.5));
#7491=CARTESIAN_POINT('Ctrl Pts',(60.599437436742,57.9223618302896,2.5));
#7492=CARTESIAN_POINT('Ctrl Pts',(60.5978171938089,57.8882030869104,2.5000000000006));
#7493=CARTESIAN_POINT('Ctrl Pts',(60.5927186872873,57.8544686959723,2.50350008622548));
#7494=CARTESIAN_POINT('Ctrl Pts',(60.5724543137635,57.7744341680499,2.51995587221184));
#7495=CARTESIAN_POINT('Ctrl Pts',(60.5542720230614,57.7307439456104,2.53604375043265));
#7496=CARTESIAN_POINT('Ctrl Pts',(60.5033113035838,57.6412749470984,2.58265302130619));
#7497=CARTESIAN_POINT('Ctrl Pts',(60.468199991714,57.5985821334833,2.61563853552051));
#7498=CARTESIAN_POINT('Ctrl Pts',(60.3812501918168,57.5182917420486,2.69848124863954));
#7499=CARTESIAN_POINT('Ctrl Pts',(60.3268065827902,57.4846962962049,2.75111321481755));
#7500=CARTESIAN_POINT('Ctrl Pts',(60.2161905779354,57.439110580143,2.85912621876381));
#7501=CARTESIAN_POINT('Ctrl Pts',(60.1591133854132,57.4263552929677,2.91537316519053));
#7502=CARTESIAN_POINT('Ctrl Pts',(60.1016271094397,57.4231168880088,2.97252012062051));
#7503=CARTESIAN_POINT('Ctrl Pts',(60.1008135540976,57.4230730234755,2.9733289755364));
#7504=CARTESIAN_POINT('Ctrl Pts',(60.1,57.4230311248647,2.97413793103449));
#7505=CARTESIAN_POINT('',(62.4,57.9223618302983,2.5));
#7506=CARTESIAN_POINT('',(61.55,57.9223618302983,2.5));
#7507=CARTESIAN_POINT('',(62.4,57.4230311248647,2.97413793103448));
#7508=CARTESIAN_POINT('Origin',(62.4,57.9223618302983,3.));
#7509=CARTESIAN_POINT('',(61.55,57.4230311248647,2.97413793103448));
#7510=CARTESIAN_POINT('Ctrl Pts',(62.4,57.9223618302983,2.5));
#7511=CARTESIAN_POINT('Ctrl Pts',(62.4261965009078,57.9223618302983,2.5));
#7512=CARTESIAN_POINT('Ctrl Pts',(62.478328938404,57.9441410931384,2.5));
#7513=CARTESIAN_POINT('Ctrl Pts',(62.5,57.9962991365602,2.5));
#7514=CARTESIAN_POINT('Ctrl Pts',(62.5,58.0224956374681,2.5));
#7515=CARTESIAN_POINT('Ctrl Pts',(62.4,57.795774405517,2.5));
#7516=CARTESIAN_POINT('Ctrl Pts',(62.4594554081724,57.795774405517,2.5));
#7517=CARTESIAN_POINT('Ctrl Pts',(62.5778299501554,57.8438930222843,2.50003956285446));
#7518=CARTESIAN_POINT('Ctrl Pts',(62.6297629272325,57.9620363623577,2.50003670134987));
#7519=CARTESIAN_POINT('Ctrl Pts',(62.6308996938996,58.0224956374681,2.5));
#7520=CARTESIAN_POINT('Ctrl Pts',(62.4,57.5435955938278,2.60110845458278));
#7521=CARTESIAN_POINT('Ctrl Pts',(62.525465808539,57.5435955938278,2.60110845458278));
#7522=CARTESIAN_POINT('Ctrl Pts',(62.7758577213737,57.6445359736439,2.60266629871633));
#7523=CARTESIAN_POINT('Ctrl Pts',(62.8882033396179,57.894111688535,2.60651315196505));
#7524=CARTESIAN_POINT('Ctrl Pts',(62.8915113750724,58.022495637468,2.60848862492761));
#7525=CARTESIAN_POINT('Ctrl Pts',(62.4,57.4295787502844,2.84771995480428));
#7526=CARTESIAN_POINT('Ctrl Pts',(62.5556992155405,57.4295787502844,2.84771995480428));
#7527=CARTESIAN_POINT('Ctrl Pts',(62.8653122771054,57.5564472161643,2.85232975672316));
#7528=CARTESIAN_POINT('Ctrl Pts',(62.9981917732878,57.865391076578,2.86346859141159));
#7529=CARTESIAN_POINT('Ctrl Pts',(63.,58.0224956374681,2.86910030610042));
#7530=CARTESIAN_POINT('Ctrl Pts',(62.4,57.4230311248647,2.97413793103449));
#7531=CARTESIAN_POINT('Ctrl Pts',(62.5571790054469,57.4230311248647,2.97413793103449));
#7532=CARTESIAN_POINT('Ctrl Pts',(62.8699736304242,57.5534146323498,2.9797755837571));
#7533=CARTESIAN_POINT('Ctrl Pts',(63.,57.8656658555809,2.99324572584077));
#7534=CARTESIAN_POINT('Ctrl Pts',(63.,58.0224956374681,3.));
#7535=CARTESIAN_POINT('',(62.5,58.0224956374681,2.5));
#7536=CARTESIAN_POINT('',(63.,58.0224956374681,3.));
#7537=CARTESIAN_POINT('Origin',(62.5,58.0224956374681,3.));
#7538=CARTESIAN_POINT('Ctrl Pts',(63.,58.0224956374681,3.));
#7539=CARTESIAN_POINT('Ctrl Pts',(63.,57.8656658555809,2.99324572584077));
#7540=CARTESIAN_POINT('Ctrl Pts',(62.8699736304242,57.5534146323498,2.9797755837571));
#7541=CARTESIAN_POINT('Ctrl Pts',(62.5571790054469,57.4230311248647,2.97413793103449));
#7542=CARTESIAN_POINT('Ctrl Pts',(62.4,57.4230311248647,2.97413793103449));
#7543=CARTESIAN_POINT('Ctrl Pts',(62.4,57.9223618302983,2.5));
#7544=CARTESIAN_POINT('Ctrl Pts',(62.4261965009078,57.9223618302983,2.5));
#7545=CARTESIAN_POINT('Ctrl Pts',(62.478328938404,57.9441410931384,2.5));
#7546=CARTESIAN_POINT('Ctrl Pts',(62.5,57.9962991365602,2.5));
#7547=CARTESIAN_POINT('Ctrl Pts',(62.5,58.0224956374681,2.5));
#7548=CARTESIAN_POINT('Origin',(62.5,58.25,3.));
#7549=CARTESIAN_POINT('',(62.5,59.8248276219832,2.5));
#7550=CARTESIAN_POINT('',(63.,59.8248276219832,3.));
#7551=CARTESIAN_POINT('Origin',(62.5,59.8248276219832,3.));
#7552=CARTESIAN_POINT('',(63.,58.25,3.));
#7553=CARTESIAN_POINT('',(62.5,58.25,2.5));
#7554=CARTESIAN_POINT('Ctrl Pts',(62.5,59.8248276219832,2.5));
#7555=CARTESIAN_POINT('Ctrl Pts',(62.5,59.8510230353731,2.5));
#7556=CARTESIAN_POINT('Ctrl Pts',(62.4783243250786,59.9031804190904,2.5));
#7557=CARTESIAN_POINT('Ctrl Pts',(62.4261954133899,59.9249530663145,2.5));
#7558=CARTESIAN_POINT('Ctrl Pts',(62.4,59.9249530663145,2.5));
#7559=CARTESIAN_POINT('Ctrl Pts',(62.6308996938996,59.8248276219832,2.5));
#7560=CARTESIAN_POINT('Ctrl Pts',(62.632002342098,59.88528980914,2.49996440019004));
#7561=CARTESIAN_POINT('Ctrl Pts',(62.5841127217071,60.0076681632058,2.49996163056113));
#7562=CARTESIAN_POINT('Ctrl Pts',(62.4616961944695,60.0600211649479,2.5));
#7563=CARTESIAN_POINT('Ctrl Pts',(62.4,60.0600211649479,2.5));
#7564=CARTESIAN_POINT('Ctrl Pts',(62.8915104141354,59.8248276219832,2.6084895858646));
#7565=CARTESIAN_POINT('Ctrl Pts',(62.8947191635119,59.9532224119501,2.61040576775692));
#7566=CARTESIAN_POINT('Ctrl Pts',(62.7941486746792,60.2153029522765,2.61426676371213));
#7567=CARTESIAN_POINT('Ctrl Pts',(62.5319883196965,60.3287554028044,2.61590736409173));
#7568=CARTESIAN_POINT('Ctrl Pts',(62.4,60.3287554028044,2.61590736409173));
#7569=CARTESIAN_POINT('Ctrl Pts',(63.,59.8248276219832,2.86910030610042));
#7570=CARTESIAN_POINT('Ctrl Pts',(63.0017539553053,59.9819463765234,2.87456299271468));
#7571=CARTESIAN_POINT('Ctrl Pts',(62.8752950337675,60.2975677764337,2.88549898701103));
#7572=CARTESIAN_POINT('Ctrl Pts',(62.5592603934469,60.4310810801322,2.89010084214396));
#7573=CARTESIAN_POINT('Ctrl Pts',(62.4,60.4310810801322,2.89010084214396));
#7574=CARTESIAN_POINT('Ctrl Pts',(63.,59.8248276219832,3.));
#7575=CARTESIAN_POINT('Ctrl Pts',(63.,59.981671565445,3.00655155402523));
#7576=CARTESIAN_POINT('Ctrl Pts',(62.8699459504713,60.2939632906984,3.01957544083796));
#7577=CARTESIAN_POINT('Ctrl Pts',(62.5571724803396,60.4243276752005,3.025));
#7578=CARTESIAN_POINT('Ctrl Pts',(62.4,60.4243276752005,3.025));
#7579=CARTESIAN_POINT('',(62.4,59.9249530663145,2.5));
#7580=CARTESIAN_POINT('',(62.4,60.4243276752005,3.025));
#7581=CARTESIAN_POINT('Origin',(62.4,59.9249530663145,3.));
#7582=CARTESIAN_POINT('Ctrl Pts',(62.4,60.4243276752005,3.025));
#7583=CARTESIAN_POINT('Ctrl Pts',(62.5571724803396,60.4243276752005,3.025));
#7584=CARTESIAN_POINT('Ctrl Pts',(62.8699459504713,60.2939632906984,3.01957544083796));
#7585=CARTESIAN_POINT('Ctrl Pts',(63.,59.981671565445,3.00655155402523));
#7586=CARTESIAN_POINT('Ctrl Pts',(63.,59.8248276219832,3.));
#7587=CARTESIAN_POINT('Ctrl Pts',(62.5,59.8248276219832,2.5));
#7588=CARTESIAN_POINT('Ctrl Pts',(62.5,59.8510230353731,2.5));
#7589=CARTESIAN_POINT('Ctrl Pts',(62.4783243250786,59.9031804190904,2.5));
#7590=CARTESIAN_POINT('Ctrl Pts',(62.4261954133899,59.9249530663145,2.5));
#7591=CARTESIAN_POINT('Ctrl Pts',(62.4,59.9249530663145,2.5));
#7592=CARTESIAN_POINT('Origin',(60.55,59.9249530663145,3.));
#7593=CARTESIAN_POINT('',(60.1,60.4243276752005,3.025));
#7594=CARTESIAN_POINT('',(60.6,59.9478721217627,2.50052555931523));
#7595=CARTESIAN_POINT('Ctrl Pts',(60.1,60.4243276752005,3.02500000000001));
#7596=CARTESIAN_POINT('Ctrl Pts',(60.1007940667368,60.4243675436247,3.02420362885053));
#7597=CARTESIAN_POINT('Ctrl Pts',(60.1015881345702,60.4244055071002,3.02340716123028));
#7598=CARTESIAN_POINT('Ctrl Pts',(60.1905412267977,60.4284448449559,2.93417456909374));
#7599=CARTESIAN_POINT('Ctrl Pts',(60.2769563903458,60.408909880705,2.84632072950434));
#7600=CARTESIAN_POINT('Ctrl Pts',(60.4115325491487,60.3362328533456,2.70762122730233));
#7601=CARTESIAN_POINT('Ctrl Pts',(60.4622024183737,60.2928539985268,2.65468544195));
#7602=CARTESIAN_POINT('Ctrl Pts',(60.5329987364422,60.2000785105811,2.5793032617521));
#7603=CARTESIAN_POINT('Ctrl Pts',(60.5587918082574,60.1527949769168,2.55124410360597));
#7604=CARTESIAN_POINT('Ctrl Pts',(60.5905898947881,60.0547893216016,2.5148548390835));
#7605=CARTESIAN_POINT('Ctrl Pts',(60.5988534347359,60.0074936809124,2.50440931235233));
#7606=CARTESIAN_POINT('Ctrl Pts',(60.5999631921872,59.9548737120598,2.50088368385959));
#7607=CARTESIAN_POINT('Ctrl Pts',(60.6,59.9513712471188,2.50068612138112));
#7608=CARTESIAN_POINT('Ctrl Pts',(60.6,59.9478721217627,2.50052555931523));
#7609=CARTESIAN_POINT('',(60.55,60.4243276752005,3.025));
#7610=CARTESIAN_POINT('',(60.6,59.9249530663145,2.5));
#7611=CARTESIAN_POINT('',(60.55,59.9249530663145,2.5));
#7612=CARTESIAN_POINT('Origin',(60.6,59.9249530663145,3.));
#7613=CARTESIAN_POINT('Origin',(62.3,59.,2.5));
#7614=CARTESIAN_POINT('',(60.6,57.9460956406901,2.5));
#7615=CARTESIAN_POINT('Ctrl Pts',(60.599437436742,57.9223618302896,2.5));
#7616=CARTESIAN_POINT('Ctrl Pts',(60.5998192566414,57.9304115416576,2.5));
#7617=CARTESIAN_POINT('Ctrl Pts',(60.6,57.9383411366579,2.5));
#7618=CARTESIAN_POINT('Ctrl Pts',(60.6,57.9460956406901,2.5));
#7619=CARTESIAN_POINT('',(60.6,61.5,2.5));
#7620=CARTESIAN_POINT('Origin',(60.1,0.,0.));
#7621=CARTESIAN_POINT('Origin',(60.6,0.,0.));
#7622=CARTESIAN_POINT('Origin',(60.1,0.,0.));
#7623=CARTESIAN_POINT('Origin',(60.6,61.5,0.));
#7624=CARTESIAN_POINT('Origin',(60.6,0.,0.));
#7625=CARTESIAN_POINT('Origin',(60.1,0.,0.));
#7626=CARTESIAN_POINT('Origin',(61.55,0.,0.));
#7627=CARTESIAN_POINT('Origin',(62.4,0.,0.));
#7628=CARTESIAN_POINT('Origin',(62.4,0.,0.));
#7629=CARTESIAN_POINT('Origin',(63.,0.,0.));
#7630=CARTESIAN_POINT('Origin',(63.,57.5,0.));
#7631=CARTESIAN_POINT('Origin',(63.,0.,0.));
#7632=CARTESIAN_POINT('Origin',(60.55,0.,0.));
#7633=CARTESIAN_POINT('',(62.4,-60.5,-7.40911313484149E-15));
#7634=CARTESIAN_POINT('Origin',(62.4,0.,0.));
#7635=CARTESIAN_POINT('',(58.9,-60.5,-7.40911313484149E-15));
#7636=CARTESIAN_POINT('',(60.55,-60.5,-7.40911313484149E-15));
#7637=CARTESIAN_POINT('',(58.9,-7.40911313484149E-15,60.5));
#7638=CARTESIAN_POINT('Origin',(58.9,0.,0.));
#7639=CARTESIAN_POINT('Origin',(58.9,0.,0.));
#7640=CARTESIAN_POINT('Origin',(62.4,0.,0.));
#7641=CARTESIAN_POINT('Origin',(62.4,0.,0.));
#7642=CARTESIAN_POINT('Origin',(58.9,0.,0.));
#7643=CARTESIAN_POINT('Origin',(58.9,-7.3111413909097E-15,59.7));
#7644=CARTESIAN_POINT('',(0.,0.,0.));
#7645=CARTESIAN_POINT('Origin',(33.5,0.,0.));
#7646=CARTESIAN_POINT('',(34.,-1.95309552664072E-15,15.9482352626124));
#7647=CARTESIAN_POINT('Origin',(34.,0.,0.));
#7648=CARTESIAN_POINT('',(33.9893953126264,-1.9656397769387E-15,16.0506668396737));
#7649=CARTESIAN_POINT('Origin',(33.5,-1.95309552664072E-15,15.9482352626124));
#7650=CARTESIAN_POINT('',(33.9893953126264,-16.0506668396737,-1.96563977693869E-15));
#7651=CARTESIAN_POINT('Origin',(33.9893953126264,0.,-2.45704972117337E-15));
#7652=CARTESIAN_POINT('Origin',(33.9893953126264,0.,-2.45704972117337E-15));
#7653=CARTESIAN_POINT('Origin',(29.5,0.,0.));
#7654=CARTESIAN_POINT('',(25.0305152653967,-58.8542048431045,-7.20756135774706E-15));
#7655=CARTESIAN_POINT('',(29.5,-37.5,-4.59242549680258E-15));
#7656=CARTESIAN_POINT('',(25.0305152653967,-7.20756135774706E-15,58.8542048431045));
#7657=CARTESIAN_POINT('Origin',(25.0305152653967,0.,-9.00945169718383E-15));
#7658=CARTESIAN_POINT('Origin',(25.0305152653967,0.,-9.00945169718383E-15));
#7659=CARTESIAN_POINT('Origin',(34.,10.5,0.));
#7660=CARTESIAN_POINT('',(34.,-1.34711147906209E-15,11.));
#7661=CARTESIAN_POINT('Origin',(34.,0.,0.));
#7662=CARTESIAN_POINT('Origin',(24.5411199527703,0.,0.));
#7663=CARTESIAN_POINT('',(24.8946733433636,-7.23831491026085E-15,59.1053266566364));
#7664=CARTESIAN_POINT('Origin',(24.5411199527703,-7.19501710744908E-15,
58.7517732660432));
#7665=CARTESIAN_POINT('',(24.8946733433636,-59.1053266566364,-7.23831491026085E-15));
#7666=CARTESIAN_POINT('Origin',(24.8946733433636,0.,-9.04789363782607E-15));
#7667=CARTESIAN_POINT('Origin',(24.8946733433636,0.,-9.04789363782607E-15));
#7668=CARTESIAN_POINT('Origin',(24.75,0.,0.));
#7669=CARTESIAN_POINT('',(24.6464466094067,-59.3535533905933,-7.26871391778116E-15));
#7670=CARTESIAN_POINT('',(24.75,-59.25,-7.25603228494807E-15));
#7671=CARTESIAN_POINT('',(24.6464466094067,-7.26871391778116E-15,59.3535533905933));
#7672=CARTESIAN_POINT('Origin',(24.6464466094067,0.,-9.08589239722645E-15));
#7673=CARTESIAN_POINT('Origin',(24.6464466094067,0.,-9.08589239722645E-15));
#7674=CARTESIAN_POINT('Origin',(24.2928932188135,0.,0.));
#7675=CARTESIAN_POINT('',(24.2928932188135,-7.28664845492675E-15,59.5));
#7676=CARTESIAN_POINT('Origin',(24.2928932188135,-7.22541611496938E-15,
59.));
#7677=CARTESIAN_POINT('',(24.2928932188135,-59.5,-7.28664845492675E-15));
#7678=CARTESIAN_POINT('Origin',(24.2928932188135,0.,0.));
#7679=CARTESIAN_POINT('Origin',(24.2928932188135,0.,0.));
#7680=CARTESIAN_POINT('Origin',(23.8,0.,0.));
#7681=CARTESIAN_POINT('',(23.3071067811865,-59.5,-7.28664845492675E-15));
#7682=CARTESIAN_POINT('',(23.8,-59.5,-7.28664845492675E-15));
#7683=CARTESIAN_POINT('',(23.3071067811865,-7.28664845492675E-15,59.5));
#7684=CARTESIAN_POINT('Origin',(23.3071067811865,0.,0.));
#7685=CARTESIAN_POINT('Origin',(23.3071067811865,0.,0.));
#7686=CARTESIAN_POINT('Origin',(23.3071067811865,0.,0.));
#7687=CARTESIAN_POINT('',(22.9535533905933,-7.26871391778116E-15,59.3535533905933));
#7688=CARTESIAN_POINT('Origin',(23.3071067811865,-7.22541611496938E-15,
59.));
#7689=CARTESIAN_POINT('',(22.9535533905933,-59.3535533905933,-7.26871391778116E-15));
#7690=CARTESIAN_POINT('Origin',(22.9535533905933,0.,-9.08589239722645E-15));
#7691=CARTESIAN_POINT('Origin',(22.9535533905933,0.,-9.08589239722645E-15));
#7692=CARTESIAN_POINT('Origin',(22.85,0.,0.));
#7693=CARTESIAN_POINT('',(22.711396327342,-59.111396327342,-7.239058230541E-15));
#7694=CARTESIAN_POINT('',(22.85,-59.25,-7.25603228494807E-15));
#7695=CARTESIAN_POINT('',(22.711396327342,-7.239058230541E-15,59.111396327342));
#7696=CARTESIAN_POINT('Origin',(22.711396327342,0.,-9.04882278817625E-15));
#7697=CARTESIAN_POINT('Origin',(22.711396327342,0.,-9.04882278817625E-15));
#7698=CARTESIAN_POINT('Origin',(23.0649497179352,0.,0.));
#7699=CARTESIAN_POINT('',(22.5725810104247,-7.20641770909798E-15,58.8448662431924));
#7700=CARTESIAN_POINT('Origin',(23.0649497179352,-7.19576042772922E-15,
58.7578429367487));
#7701=CARTESIAN_POINT('',(22.5725810104247,-58.8448662431925,-7.20641770909798E-15));
#7702=CARTESIAN_POINT('Origin',(22.5725810104247,0.,-9.00802213637247E-15));
#7703=CARTESIAN_POINT('Origin',(22.5725810104247,0.,-9.00802213637247E-15));
#7704=CARTESIAN_POINT('Origin',(18.8,0.,0.));
#7705=CARTESIAN_POINT('',(15.0076312924895,-16.0431770496114,-1.96472254219609E-15));
#7706=CARTESIAN_POINT('',(18.8,-37.5,-4.59242549680258E-15));
#7707=CARTESIAN_POINT('',(15.0076312924895,-1.96472254219609E-15,16.0431770496114));
#7708=CARTESIAN_POINT('Origin',(15.0076312924895,0.,-2.45590317774511E-15));
#7709=CARTESIAN_POINT('Origin',(15.0076312924895,0.,-2.45590317774511E-15));
#7710=CARTESIAN_POINT('Origin',(15.5,0.,0.));
#7711=CARTESIAN_POINT('',(15.,-1.95406526082734E-15,15.9561537431677));
#7712=CARTESIAN_POINT('Origin',(15.5,-1.95406526082734E-15,15.9561537431677));
#7713=CARTESIAN_POINT('Origin',(15.,0.,0.));
#7714=CARTESIAN_POINT('Origin',(15.,16.,0.));
#7715=CARTESIAN_POINT('',(15.,-1.34711147906209E-15,11.));
#7716=CARTESIAN_POINT('Origin',(15.,0.,0.));
#7717=CARTESIAN_POINT('Origin',(15.5,0.,0.));
#7718=CARTESIAN_POINT('',(15.5,-1.28587913910472E-15,10.5));
#7719=CARTESIAN_POINT('Origin',(15.5,-1.34711147906209E-15,11.));
#7720=CARTESIAN_POINT('',(15.5,-10.5,-1.28587913910472E-15));
#7721=CARTESIAN_POINT('Origin',(15.5,0.,0.));
#7722=CARTESIAN_POINT('Origin',(15.5,0.,0.));
#7723=CARTESIAN_POINT('Origin',(24.5,0.,0.));
#7724=CARTESIAN_POINT('',(33.5,-1.28587913910472E-15,10.5));
#7725=CARTESIAN_POINT('',(33.5,-10.5,-1.28587913910472E-15));
#7726=CARTESIAN_POINT('Origin',(33.5,0.,0.));
#7727=CARTESIAN_POINT('Origin',(33.5,0.,0.));
#7728=CARTESIAN_POINT('',(24.5,-10.5,-1.28587913910472E-15));
#7729=CARTESIAN_POINT('Origin',(33.5,0.,0.));
#7730=CARTESIAN_POINT('Origin',(33.5,-1.34711147906209E-15,11.));
#7731=CARTESIAN_POINT('',(0.,0.,0.));
#7732=CARTESIAN_POINT('Origin',(84.65,0.,0.));
#7733=CARTESIAN_POINT('',(92.9209088298366,-3.45967356244292,-0.00100989411776997));
#7734=CARTESIAN_POINT('',(93.2183732864721,-3.44877006476889,0.000221723780192462));
#7735=CARTESIAN_POINT('',(84.65,-3.4544,-4.23041990297462E-16));
#7736=CARTESIAN_POINT('',(93.8044,3.25944077490411,1.14408268708712));
#7737=CARTESIAN_POINT('Ctrl Pts',(93.2183732864721,-3.44877006476889,0.000221723780192462));
#7738=CARTESIAN_POINT('Ctrl Pts',(93.2462262172957,-3.448754724225,-0.573040469566619));
#7739=CARTESIAN_POINT('Ctrl Pts',(93.2740791481193,-3.31345071435984,-1.14634497961049));
#7740=CARTESIAN_POINT('Ctrl Pts',(93.3019320789429,-3.04283652130647,-1.64659870953629));
#7741=CARTESIAN_POINT('Ctrl Pts',(93.3577618479492,-2.50040427301956,-2.64933161269944));
#7742=CARTESIAN_POINT('Ctrl Pts',(93.4135916169555,-1.41432083486459,-3.35856004638195));
#7743=CARTESIAN_POINT('Ctrl Pts',(93.4694213859618,-0.277922290246916,-3.44943135077171));
#7744=CARTESIAN_POINT('Ctrl Pts',(93.5252511549682,0.858476254370759,-3.54030265516147));
#7745=CARTESIAN_POINT('Ctrl Pts',(93.5810809239746,2.04518990545115,-3.01281683025845));
#7746=CARTESIAN_POINT('Ctrl Pts',(93.636910692981,2.74023372258513,-2.11180914044543));
#7747=CARTESIAN_POINT('Ctrl Pts',(93.6927404619873,3.43527753971911,-1.21080145063241));
#7748=CARTESIAN_POINT('Ctrl Pts',(93.7485702309937,3.6386515229067,0.063728104090605));
#7749=CARTESIAN_POINT('Ctrl Pts',(93.8044,3.25944077490411,1.14408268708712));
#7750=CARTESIAN_POINT('',(93.8044,-1.75208009336914,2.97731016051328));
#7751=CARTESIAN_POINT('Origin',(93.8044,0.,0.));
#7752=CARTESIAN_POINT('Ctrl Pts',(93.8044,-1.75208009336914,2.97731016051328));
#7753=CARTESIAN_POINT('Ctrl Pts',(93.7917271656399,-1.52951455720307,3.11157965083414));
#7754=CARTESIAN_POINT('Ctrl Pts',(93.7790543312797,-1.2925249415104,3.22041651535433));
#7755=CARTESIAN_POINT('Ctrl Pts',(93.7663814969195,-1.04589844408296,3.2987746062456));
#7756=CARTESIAN_POINT('Ctrl Pts',(93.7105517279132,0.0406067520640256,3.64397868529463));
#7757=CARTESIAN_POINT('Ctrl Pts',(93.6547219589068,1.31414599657454,3.39764614722317));
#7758=CARTESIAN_POINT('Ctrl Pts',(93.5988921899005,2.19521568785426,2.67416693511821));
#7759=CARTESIAN_POINT('Ctrl Pts',(93.5430624208941,3.07628537913397,1.95068772301326));
#7760=CARTESIAN_POINT('Ctrl Pts',(93.4872326518878,3.56488551718289,0.750061836874816));
#7761=CARTESIAN_POINT('Ctrl Pts',(93.4314028828814,3.43877773600297,-0.382618805547265));
#7762=CARTESIAN_POINT('Ctrl Pts',(93.3755731138751,3.31266995482305,-1.51529944796938));
#7763=CARTESIAN_POINT('Ctrl Pts',(93.3197433448686,2.57185425441423,-2.58003484667512));
#7764=CARTESIAN_POINT('Ctrl Pts',(93.2639135758623,1.55334430498576,-3.09183132689595));
#7765=CARTESIAN_POINT('Ctrl Pts',(93.2080838068559,0.534834355557293,-3.60362780711678));
#7766=CARTESIAN_POINT('Ctrl Pts',(93.1522540378496,-0.761369842890835,-3.5624853688527));
#7767=CARTESIAN_POINT('Ctrl Pts',(93.0964242688433,-1.74552965897778,-2.98741603452504));
#7768=CARTESIAN_POINT('Ctrl Pts',(93.0405944998369,-2.72968947506471,-2.41234670019739));
#7769=CARTESIAN_POINT('Ctrl Pts',(92.9847647308305,-3.40180490879047,-1.30335046980618));
#7770=CARTESIAN_POINT('Ctrl Pts',(92.9289349618241,-3.45609656090976,-0.164829487232134));
#7771=CARTESIAN_POINT('Ctrl Pts',(92.9262595844949,-3.45869823127002,-0.110271259967334));
#7772=CARTESIAN_POINT('Ctrl Pts',(92.9235842071657,-3.45988116087502,-0.0556452334846064));
#7773=CARTESIAN_POINT('Ctrl Pts',(92.9209088298366,-3.45967356244292,-0.00100989411776997));
#7774=CARTESIAN_POINT('Origin',(84.65,0.,0.));
#7775=CARTESIAN_POINT('',(91.8625754965033,-3.45043530540852,-0.00223112594461949));
#7776=CARTESIAN_POINT('',(92.1600399531387,-3.45616980202756,0.00289452556765842));
#7777=CARTESIAN_POINT('',(84.65,-3.4544,-4.23041990297462E-16));
#7778=CARTESIAN_POINT('Ctrl Pts',(92.1600399531387,-3.45616980202756,0.00289452556765842));
#7779=CARTESIAN_POINT('Ctrl Pts',(92.2056920477019,-3.44779680921498,-0.931879971447121));
#7780=CARTESIAN_POINT('Ctrl Pts',(92.2513441422651,-3.05497186656688,-1.87285172139297));
#7781=CARTESIAN_POINT('Ctrl Pts',(92.2969962368283,-2.37792145309273,-2.51340958946608));
#7782=CARTESIAN_POINT('Ctrl Pts',(92.3528260058347,-1.54992947262409,-3.29677337927473));
#7783=CARTESIAN_POINT('Ctrl Pts',(92.408655774841,-0.296854978392081,-3.63084355825839));
#7784=CARTESIAN_POINT('Ctrl Pts',(92.4644855438474,0.811213403585058,-3.36359464588894));
#7785=CARTESIAN_POINT('Ctrl Pts',(92.5203153128537,1.91928178556216,-3.0963457335195));
#7786=CARTESIAN_POINT('Ctrl Pts',(92.5761450818601,2.88234405528443,-2.22777772979697));
#7787=CARTESIAN_POINT('Ctrl Pts',(92.6319748508664,3.26221848023226,-1.15312751939853));
#7788=CARTESIAN_POINT('Ctrl Pts',(92.6878046198728,3.6420929051801,-0.0784773090000682));
#7789=CARTESIAN_POINT('Ctrl Pts',(92.7436343888792,3.43877948535351,1.20225510807429));
#7790=CARTESIAN_POINT('Ctrl Pts',(92.7994641578856,2.74482734879403,2.10652594559603));
#7791=CARTESIAN_POINT('Ctrl Pts',(92.855293926892,2.05087521223453,3.0107967831178));
#7792=CARTESIAN_POINT('Ctrl Pts',(92.9111236958982,0.86628435894208,3.53860604108688));
#7793=CARTESIAN_POINT('Ctrl Pts',(92.9669534649046,-0.270098466384267,3.44954294338115));
#7794=CARTESIAN_POINT('Ctrl Pts',(93.0227832339109,-1.40648129171058,3.36047984567542));
#7795=CARTESIAN_POINT('Ctrl Pts',(93.0786130029174,-2.49465608907082,2.65454439229492));
#7796=CARTESIAN_POINT('Ctrl Pts',(93.1344427719237,-3.03935295854151,1.65345797928278));
#7797=CARTESIAN_POINT('Ctrl Pts',(93.1624196101066,-3.31230583739212,1.15180387821292));
#7798=CARTESIAN_POINT('Ctrl Pts',(93.1903964482893,-3.44878547355717,0.576034148015107));
#7799=CARTESIAN_POINT('Ctrl Pts',(93.2183732864721,-3.44877006476889,0.000221723780192462));
#7800=CARTESIAN_POINT('Ctrl Pts',(92.9209088298366,-3.45967356244292,-0.00100989411776997));
#7801=CARTESIAN_POINT('Ctrl Pts',(92.8677544381594,-3.45554899718949,1.08448492428777));
#7802=CARTESIAN_POINT('Ctrl Pts',(92.8146000464823,-2.902531081883,2.17365588587066));
#7803=CARTESIAN_POINT('Ctrl Pts',(92.7614456548051,-2.02188203340776,2.80781567790935));
#7804=CARTESIAN_POINT('Ctrl Pts',(92.7056158857987,-1.09690798327364,3.47389412571991));
#7805=CARTESIAN_POINT('Ctrl Pts',(92.6497861167924,0.189507987507439,3.63800528658412));
#7806=CARTESIAN_POINT('Ctrl Pts',(92.593956347786,1.25209352043107,3.22552316675482));
#7807=CARTESIAN_POINT('Ctrl Pts',(92.5381265787796,2.31467905335469,2.81304104692552));
#7808=CARTESIAN_POINT('Ctrl Pts',(92.4822968097733,3.15343414842088,1.82396564640271));
#7809=CARTESIAN_POINT('Ctrl Pts',(92.4264670407669,3.38675808805357,0.708269247798187));
#7810=CARTESIAN_POINT('Ctrl Pts',(92.3706372717606,3.62008202768626,-0.407427150806336));
#7811=CARTESIAN_POINT('Ctrl Pts',(92.3148075027542,3.24797481188544,-1.64974454749257));
#7812=CARTESIAN_POINT('Ctrl Pts',(92.2589777337479,2.43973058675324,-2.45346584442737));
#7813=CARTESIAN_POINT('Ctrl Pts',(92.2031479647415,1.63148636162103,-3.25718714136217));
#7814=CARTESIAN_POINT('Ctrl Pts',(92.1473181957351,0.387105127157411,-3.62231233854551));
#7815=CARTESIAN_POINT('Ctrl Pts',(92.0914884267288,-0.727266665982812,-3.38272834733937));
#7816=CARTESIAN_POINT('Ctrl Pts',(92.0356586577225,-1.84163845912302,-3.14314435613323));
#7817=CARTESIAN_POINT('Ctrl Pts',(91.9798288887161,-2.82600081093984,-2.29885117653763));
#7818=CARTESIAN_POINT('Ctrl Pts',(91.9239991197097,-3.23250637058094,-1.23396759562083));
#7819=CARTESIAN_POINT('Ctrl Pts',(91.9035245786409,-3.38158480890701,-0.843441125620498));
#7820=CARTESIAN_POINT('Ctrl Pts',(91.8830500375721,-3.45294608894601,-0.423246995105974));
#7821=CARTESIAN_POINT('Ctrl Pts',(91.8625754965033,-3.45043530540852,-0.00223112594461949));
#7822=CARTESIAN_POINT('Origin',(84.65,0.,0.));
#7823=CARTESIAN_POINT('',(90.80424216317,-3.45180239605614,0.00279451803522027));
#7824=CARTESIAN_POINT('',(91.1017066198054,-3.45763635249975,-0.00244580608254598));
#7825=CARTESIAN_POINT('',(84.65,-3.4544,-4.23041990297462E-16));
#7826=CARTESIAN_POINT('Ctrl Pts',(91.1017066198054,-3.45763635249975,-0.00244580608254598));
#7827=CARTESIAN_POINT('Ctrl Pts',(91.1093281091019,-3.45888988877411,-0.158332497209808));
#7828=CARTESIAN_POINT('Ctrl Pts',(91.1169495983983,-3.44925346319397,-0.314063335739518));
#7829=CARTESIAN_POINT('Ctrl Pts',(91.1245710876948,-3.428196288038,-0.468234288642407));
#7830=CARTESIAN_POINT('Ctrl Pts',(91.1804008567011,-3.27394595989943,-1.59758425598427));
#7831=CARTESIAN_POINT('Ctrl Pts',(91.2362306257075,-2.50685636728464,-2.64323050897187));
#7832=CARTESIAN_POINT('Ctrl Pts',(91.2920603947139,-1.47592424748071,-3.12944403336781));
#7833=CARTESIAN_POINT('Ctrl Pts',(91.3478901637202,-0.444992127676794,-3.61565755776375));
#7834=CARTESIAN_POINT('Ctrl Pts',(91.4037199327265,0.849782519316258,-3.54243835356805));
#7835=CARTESIAN_POINT('Ctrl Pts',(91.4595497017329,1.81932662547287,-2.94309775990678));
#7836=CARTESIAN_POINT('Ctrl Pts',(91.5153794707393,2.78887073162951,-2.3437571662455));
#7837=CARTESIAN_POINT('Ctrl Pts',(91.5712092397457,3.43318429694969,-1.21829518311862));
#7838=CARTESIAN_POINT('Ctrl Pts',(91.6270390087521,3.45912869688117,-0.0787554811289303));
#7839=CARTESIAN_POINT('Ctrl Pts',(91.6828687777584,3.48507309681266,1.06078422086078));
#7840=CARTESIAN_POINT('Ctrl Pts',(91.7386985467648,2.89264833135546,2.21440164171326));
#7841=CARTESIAN_POINT('Ctrl Pts',(91.7945283157711,1.9513860055696,2.85724707365223));
#7842=CARTESIAN_POINT('Ctrl Pts',(91.8503580847774,1.01012367978377,3.50009250559118));
#7843=CARTESIAN_POINT('Ctrl Pts',(91.9061878537838,-0.279976206330739,3.6321659486166));
#7844=CARTESIAN_POINT('Ctrl Pts',(91.9620176227901,-1.33196886180909,3.19337427179059));
#7845=CARTESIAN_POINT('Ctrl Pts',(92.0178473917965,-2.38396151728742,2.75458259496459));
#7846=CARTESIAN_POINT('Ctrl Pts',(92.0736771608029,-3.19784694212965,1.7449257982872));
#7847=CARTESIAN_POINT('Ctrl Pts',(92.1295069298093,-3.40333492119814,0.623768699631705));
#7848=CARTESIAN_POINT('Ctrl Pts',(92.1396846042524,-3.44079503952147,0.419383617034329));
#7849=CARTESIAN_POINT('Ctrl Pts',(92.1498622786956,-3.45803647639982,0.211293079881917));
#7850=CARTESIAN_POINT('Ctrl Pts',(92.1600399531387,-3.45616980202756,0.00289452556765842));
#7851=CARTESIAN_POINT('Ctrl Pts',(91.8625754965033,-3.45043530540852,-0.00223112594461949));
#7852=CARTESIAN_POINT('Ctrl Pts',(91.8272202685657,-3.44609971009669,0.724774767349627));
#7853=CARTESIAN_POINT('Ctrl Pts',(91.7918650406282,-3.22149218222548,1.45423092331462));
#7854=CARTESIAN_POINT('Ctrl Pts',(91.7565098126906,-2.7964109095389,2.03761122757244));
#7855=CARTESIAN_POINT('Ctrl Pts',(91.7006800436842,-2.12516112139035,2.95883248761094));
#7856=CARTESIAN_POINT('Ctrl Pts',(91.6448502746779,-0.954012777627767,3.51580102544994));
#7857=CARTESIAN_POINT('Ctrl Pts',(91.5890205056715,0.184206076595443,3.45511796588552));
#7858=CARTESIAN_POINT('Ctrl Pts',(91.5331907366652,1.32242493081865,3.3944349063211));
#7859=CARTESIAN_POINT('Ctrl Pts',(91.4773609676588,2.42771429550253,2.71610024935329));
#7860=CARTESIAN_POINT('Ctrl Pts',(91.4215311986524,2.99720950963122,1.72873016655719));
#7861=CARTESIAN_POINT('Ctrl Pts',(91.3657014296461,3.56670472375992,0.741360083761087));
#7862=CARTESIAN_POINT('Ctrl Pts',(91.3098716606398,3.60040578733339,-0.555045424863321));
#7863=CARTESIAN_POINT('Ctrl Pts',(91.2540418916334,3.08297998794191,-1.57067092694823));
#7864=CARTESIAN_POINT('Ctrl Pts',(91.198212122627,2.56555418855044,-2.58629642903311));
#7865=CARTESIAN_POINT('Ctrl Pts',(91.1423823536206,1.49700152619402,-3.32114192457851));
#7866=CARTESIAN_POINT('Ctrl Pts',(91.0865525846143,0.363472878981578,-3.44088071064219));
#7867=CARTESIAN_POINT('Ctrl Pts',(91.0307228156079,-0.770055768230898,-3.56061949670588));
#7868=CARTESIAN_POINT('Ctrl Pts',(90.9748930466016,-1.9685604002994,-3.06525157328782));
#7869=CARTESIAN_POINT('Ctrl Pts',(90.9190632775953,-2.68676693551405,-2.18015048631885));
#7870=CARTESIAN_POINT('Ctrl Pts',(90.8807895727868,-3.1791283657962,-1.57337567189296));
#7871=CARTESIAN_POINT('Ctrl Pts',(90.8425158679784,-3.44576451119845,-0.783438296661764));
#7872=CARTESIAN_POINT('Ctrl Pts',(90.80424216317,-3.45180239605614,0.00279451803522027));
#7873=CARTESIAN_POINT('Origin',(84.65,0.,0.));
#7874=CARTESIAN_POINT('',(89.7459088298366,-3.46002183154878,-9.14716326361198E-5));
#7875=CARTESIAN_POINT('',(90.043373286472,-3.44903894306056,-0.000821802180914491));
#7876=CARTESIAN_POINT('',(84.65,-3.4544,-4.23041990297462E-16));
#7877=CARTESIAN_POINT('Ctrl Pts',(90.043373286472,-3.44903894306056,-0.000821802180914491));
#7878=CARTESIAN_POINT('Ctrl Pts',(90.0687939395081,-3.45015973575754,-0.524074439861875));
#7879=CARTESIAN_POINT('Ctrl Pts',(90.0942145925442,-3.33844059682494,-1.04687294234206));
#7880=CARTESIAN_POINT('Ctrl Pts',(90.1196352455803,-3.11140810631006,-1.51357609271899));
#7881=CARTESIAN_POINT('Ctrl Pts',(90.1754650145866,-2.61279103756708,-2.5385666404873));
#7882=CARTESIAN_POINT('Ctrl Pts',(90.2312947835931,-1.55796517491713,-3.29298376627957));
#7883=CARTESIAN_POINT('Ctrl Pts',(90.2871245525994,-0.426836221514585,-3.43359633877573));
#7884=CARTESIAN_POINT('Ctrl Pts',(90.3429543216058,0.704292731887955,-3.57420891127189));
#7885=CARTESIAN_POINT('Ctrl Pts',(90.3987840906121,1.91172477604308,-3.10101693047194));
#7886=CARTESIAN_POINT('Ctrl Pts',(90.4546138596185,2.64612419731206,-2.22930476351716));
#7887=CARTESIAN_POINT('Ctrl Pts',(90.5104436286248,3.38052361858102,-1.35759259656241));
#7888=CARTESIAN_POINT('Ctrl Pts',(90.5662733976312,3.64189041696387,-0.0873602434528473));
#7889=CARTESIAN_POINT('Ctrl Pts',(90.6221031666375,3.31131261962515,1.0034848025557));
#7890=CARTESIAN_POINT('Ctrl Pts',(90.6779329356439,2.98073482228642,2.09432984856429));
#7891=CARTESIAN_POINT('Ctrl Pts',(90.7337627046502,2.05821242922608,3.00578758747185));
#7892=CARTESIAN_POINT('Ctrl Pts',(90.7895924736566,0.963458102751407,3.32317940954435));
#7893=CARTESIAN_POINT('Ctrl Pts',(90.845422242663,-0.131296223723232,3.64057123161685));
#7894=CARTESIAN_POINT('Ctrl Pts',(90.9012520116694,-1.39828248361219,3.36389713685432));
#7895=CARTESIAN_POINT('Ctrl Pts',(90.9570817806757,-2.26107008172552,2.61903324862501));
#7896=CARTESIAN_POINT('Ctrl Pts',(91.0052900603856,-3.00607595583795,1.97585296490451));
#7897=CARTESIAN_POINT('Ctrl Pts',(91.0534983400955,-3.44970734742079,0.983585783884964));
#7898=CARTESIAN_POINT('Ctrl Pts',(91.1017066198054,-3.45763635249975,-0.00244580608254598));
#7899=CARTESIAN_POINT('Ctrl Pts',(90.80424216317,-3.45180239605614,0.00279451803522027));
#7900=CARTESIAN_POINT('Ctrl Pts',(90.786686098972,-3.45457196055772,0.363437780515883));
#7901=CARTESIAN_POINT('Ctrl Pts',(90.7691300347741,-3.40251069416784,0.723301589857626));
#7902=CARTESIAN_POINT('Ctrl Pts',(90.7515739705762,-3.29225294667203,1.06435108224323));
#7903=CARTESIAN_POINT('Ctrl Pts',(90.6957442015698,-2.9416239842546,2.14891731331652));
#7904=CARTESIAN_POINT('Ctrl Pts',(90.6399144325634,-2.00245762105894,3.04321552494328));
#7905=CARTESIAN_POINT('Ctrl Pts',(90.584084663557,-0.902038879867245,3.34037401075845));
#7906=CARTESIAN_POINT('Ctrl Pts',(90.5282548945507,0.198379861324493,3.63753249657364));
#7907=CARTESIAN_POINT('Ctrl Pts',(90.4724251255444,1.46005098051228,3.33755125657718));
#7908=CARTESIAN_POINT('Ctrl Pts',(90.416595356538,2.30896204172667,2.57691035490764));
#7909=CARTESIAN_POINT('Ctrl Pts',(90.3607655875317,3.15787310294103,1.81626945323814));
#7910=CARTESIAN_POINT('Ctrl Pts',(90.3049358185253,3.59402410618203,0.594968889895604));
#7911=CARTESIAN_POINT('Ctrl Pts',(90.2491060495189,3.41898291147,-0.53134596547945));
#7912=CARTESIAN_POINT('Ctrl Pts',(90.1932762805125,3.24394171675795,-1.65766082085454));
#7913=CARTESIAN_POINT('Ctrl Pts',(90.1374465115062,2.45770832409283,-2.68898996826213));
#7914=CARTESIAN_POINT('Ctrl Pts',(90.0816167424998,1.41798906313595,-3.15611782081291));
#7915=CARTESIAN_POINT('Ctrl Pts',(90.0257869734935,0.378269802179101,-3.62324567336368));
#7916=CARTESIAN_POINT('Ctrl Pts',(89.9699572044871,-0.914935327069492,-3.52617223105767));
#7917=CARTESIAN_POINT('Ctrl Pts',(89.9141274354808,-1.87326711159148,-2.90906222219465));
#7918=CARTESIAN_POINT('Ctrl Pts',(89.8582976664744,-2.83159889611351,-2.29195221333161));
#7919=CARTESIAN_POINT('Ctrl Pts',(89.802467897468,-3.4550573359089,-1.15480563791153));
#7920=CARTESIAN_POINT('Ctrl Pts',(89.7466381284617,-3.45999252212756,-0.0149809950586317));
#7921=CARTESIAN_POINT('Ctrl Pts',(89.74639502892,-3.46001401140702,-0.0100178570549767));
#7922=CARTESIAN_POINT('Ctrl Pts',(89.7461519293783,-3.46002377353189,-0.00505466827536287));
#7923=CARTESIAN_POINT('Ctrl Pts',(89.7459088298366,-3.46002183154878,-9.14716326361198E-5));
#7924=CARTESIAN_POINT('Origin',(84.65,0.,0.));
#7925=CARTESIAN_POINT('',(88.6875754965033,-3.45155207576766,-0.00271849840084493));
#7926=CARTESIAN_POINT('',(88.9850399531387,-3.454679949607,0.00309179818855912));
#7927=CARTESIAN_POINT('',(84.65,-3.4544,-4.23041990297462E-16));
#7928=CARTESIAN_POINT('Ctrl Pts',(88.9850399531387,-3.454679949607,0.00309179818855912));
#7929=CARTESIAN_POINT('Ctrl Pts',(89.0282597699144,-3.44660062115878,-0.88286530776684));
#7930=CARTESIAN_POINT('Ctrl Pts',(89.0714795866901,-3.09865605805359,-1.77446071433409));
#7931=CARTESIAN_POINT('Ctrl Pts',(89.1146994034658,-2.48454027584772,-2.40807653662655));
#7932=CARTESIAN_POINT('Ctrl Pts',(89.1705291724722,-1.6912481052297,-3.2265581415103));
#7933=CARTESIAN_POINT('Ctrl Pts',(89.2263589414785,-0.453808750692432,-3.61456155175139));
#7934=CARTESIAN_POINT('Ctrl Pts',(89.2821887104849,0.664789883977839,-3.3955599535972));
#7935=CARTESIAN_POINT('Ctrl Pts',(89.3380184794913,1.78338851864816,-3.176558355443));
#7936=CARTESIAN_POINT('Ctrl Pts',(89.3938482484977,2.78314643345148,-2.35055174889353));
#7937=CARTESIAN_POINT('Ctrl Pts',(89.449678017504,3.20921175174797,-1.2933417649389));
#7938=CARTESIAN_POINT('Ctrl Pts',(89.5055077865104,3.63527707004444,-0.236131780984317));
#7939=CARTESIAN_POINT('Ctrl Pts',(89.5613375555167,3.48764979183407,1.05228158037541));
#7940=CARTESIAN_POINT('Ctrl Pts',(89.617167324523,2.8334947211445,1.98571917811078));
#7941=CARTESIAN_POINT('Ctrl Pts',(89.6729970935294,2.17933965045492,2.91915677584617));
#7942=CARTESIAN_POINT('Ctrl Pts',(89.7288268625358,1.01865678728613,3.49761860995722));
#7943=CARTESIAN_POINT('Ctrl Pts',(89.7846566315421,-0.120487252438666,3.45792651875769));
#7944=CARTESIAN_POINT('Ctrl Pts',(89.8404864005485,-1.25963129216346,3.41823442755817));
#7945=CARTESIAN_POINT('Ctrl Pts',(89.8963161695549,-2.37723650844425,2.76038841104806));
#7946=CARTESIAN_POINT('Ctrl Pts',(89.9521459385612,-2.96483497916664,1.78368341792084));
#7947=CARTESIAN_POINT('Ctrl Pts',(89.9825550545315,-3.28488556075007,1.25169598660317));
#7948=CARTESIAN_POINT('Ctrl Pts',(90.0129641705018,-3.44769820979724,0.625112162552654));
#7949=CARTESIAN_POINT('Ctrl Pts',(90.043373286472,-3.44903894306056,-0.000821802180914491));
#7950=CARTESIAN_POINT('Ctrl Pts',(89.7459088298366,-3.46002183154878,-9.14716326361198E-5));
#7951=CARTESIAN_POINT('Ctrl Pts',(89.6903221603719,-3.45957778145935,1.13478344151281));
#7952=CARTESIAN_POINT('Ctrl Pts',(89.6347354909072,-2.8471902022148,2.27006947366597));
#7953=CARTESIAN_POINT('Ctrl Pts',(89.5791488214426,-1.89838758434876,2.8927317993208));
#7954=CARTESIAN_POINT('Ctrl Pts',(89.5233190524362,-0.945435527709273,3.51811724056172));
#7955=CARTESIAN_POINT('Ctrl Pts',(89.4674892834298,0.346880518211697,3.62638541275787));
#7956=CARTESIAN_POINT('Ctrl Pts',(89.4116595144235,1.39060583950645,3.16827840989243));
#7957=CARTESIAN_POINT('Ctrl Pts',(89.3558297454172,2.43433116080121,2.710171407027));
#7958=CARTESIAN_POINT('Ctrl Pts',(89.2999999764108,3.22946575746975,1.68568922909996));
#7959=CARTESIAN_POINT('Ctrl Pts',(89.2441702074045,3.41425359020177,0.560932353464458));
#7960=CARTESIAN_POINT('Ctrl Pts',(89.1883404383981,3.59904142293379,-0.563824522171029));
#7961=CARTESIAN_POINT('Ctrl Pts',(89.1325106693917,3.1734824917293,-1.78885609551498));
#7962=CARTESIAN_POINT('Ctrl Pts',(89.0766809003854,2.33118994597285,-2.55681953198702));
#7963=CARTESIAN_POINT('Ctrl Pts',(89.020851131379,1.4888974002164,-3.32478296845905));
#7964=CARTESIAN_POINT('Ctrl Pts',(88.9650213623726,0.229871239907982,-3.63567826805917));
#7965=CARTESIAN_POINT('Ctrl Pts',(88.9091915933663,-0.873079454520174,-3.34805987841929));
#7966=CARTESIAN_POINT('Ctrl Pts',(88.8533618243599,-1.97603014894834,-3.0604414887794));
#7967=CARTESIAN_POINT('Ctrl Pts',(88.7975320553536,-2.92290537749625,-2.17430940989949));
#7968=CARTESIAN_POINT('Ctrl Pts',(88.7417022863472,-3.28291287702557,-1.09282007907629));
#7969=CARTESIAN_POINT('Ctrl Pts',(88.7236600230659,-3.39925493262351,-0.743319882497822));
#7970=CARTESIAN_POINT('Ctrl Pts',(88.7056177597846,-3.45430685025923,-0.373417349359545));
#7971=CARTESIAN_POINT('Ctrl Pts',(88.6875754965033,-3.45155207576766,-0.00271849840084493));
#7972=CARTESIAN_POINT('Origin',(84.65,0.,0.));
#7973=CARTESIAN_POINT('',(87.6292421631699,-3.45063882513586,0.00234158759808215));
#7974=CARTESIAN_POINT('',(87.9267066198054,-3.45881529047273,-0.00181033228093454));
#7975=CARTESIAN_POINT('',(84.65,-3.4544,-4.23041990297462E-16));
#7976=CARTESIAN_POINT('Ctrl Pts',(87.9267066198054,-3.45881529047273,-0.00181033228093454));
#7977=CARTESIAN_POINT('Ctrl Pts',(87.9318958313143,-3.45949248446936,-0.107853322368814));
#7978=CARTESIAN_POINT('Ctrl Pts',(87.9370850428233,-3.45503548807332,-0.213838636952292));
#7979=CARTESIAN_POINT('Ctrl Pts',(87.9422742543323,-3.44525773166627,-0.319330785970636));
#7980=CARTESIAN_POINT('Ctrl Pts',(87.9981040233386,-3.34006065487291,-1.45430134970563));
#7981=CARTESIAN_POINT('Ctrl Pts',(88.053933792345,-2.61897437949145,-2.53218695864979));
#7982=CARTESIAN_POINT('Ctrl Pts',(88.1097635613514,-1.61006577127509,-3.06259060284673));
#7983=CARTESIAN_POINT('Ctrl Pts',(88.1655933303578,-0.601157163058717,-3.59299424704368));
#7984=CARTESIAN_POINT('Ctrl Pts',(88.2214230993641,0.695573777992526,-3.57591592649341));
#7985=CARTESIAN_POINT('Ctrl Pts',(88.2772528683704,1.69016372837544,-3.01912562834955));
#7986=CARTESIAN_POINT('Ctrl Pts',(88.3330826373768,2.68475367875835,-2.46233533020569));
#7987=CARTESIAN_POINT('Ctrl Pts',(88.3889124063832,3.37720263847291,-1.36583305446821));
#7988=CARTESIAN_POINT('Ctrl Pts',(88.4447421753896,3.45247263264309,-0.228485687350275));
#7989=CARTESIAN_POINT('Ctrl Pts',(88.5005719443959,3.52774262681328,0.908861679767659));
#7990=CARTESIAN_POINT('Ctrl Pts',(88.5564017134023,2.98583365543915,2.08705413826606));
#7991=CARTESIAN_POINT('Ctrl Pts',(88.6122314824086,2.07329371677074,2.77005887166429));
#7992=CARTESIAN_POINT('Ctrl Pts',(88.668061251415,1.16075377810231,3.45306360506253));
#7993=CARTESIAN_POINT('Ctrl Pts',(88.7238910204213,-0.122417127860435,3.64088061336055));
#7994=CARTESIAN_POINT('Ctrl Pts',(88.7797207894276,-1.19242497851517,3.24806029178481));
#7995=CARTESIAN_POINT('Ctrl Pts',(88.835550558434,-2.26243282916989,2.85523997020907));
#7996=CARTESIAN_POINT('Ctrl Pts',(88.8913803274404,-3.11927762451663,1.88178231875958));
#7997=CARTESIAN_POINT('Ctrl Pts',(88.9472100964468,-3.37312752884059,0.770573593271612));
#7998=CARTESIAN_POINT('Ctrl Pts',(88.9598200486774,-3.43046316221776,0.519591201689593));
#7999=CARTESIAN_POINT('Ctrl Pts',(88.9724300009081,-3.45703720036345,0.261581482272195));
#8000=CARTESIAN_POINT('Ctrl Pts',(88.9850399531387,-3.454679949607,0.00309179818855912));
#8001=CARTESIAN_POINT('Ctrl Pts',(88.6875754965033,-3.45155207576766,-0.00271849840084493));
#8002=CARTESIAN_POINT('Ctrl Pts',(88.6497879907782,-3.44578250821131,0.773668850262181));
#8003=CARTESIAN_POINT('Ctrl Pts',(88.6120004850532,-3.18644605389839,1.55354921717556));
#8004=CARTESIAN_POINT('Ctrl Pts',(88.5742129793281,-2.7055449759783,2.15680297346112));
#8005=CARTESIAN_POINT('Ctrl Pts',(88.5183832103217,-1.99502980489096,3.04809011240894));
#8006=CARTESIAN_POINT('Ctrl Pts',(88.4625534413154,-0.800859692205512,3.55381780753807));
#8007=CARTESIAN_POINT('Ctrl Pts',(88.4067236723091,0.333663319839212,3.44389916698642));
#8008=CARTESIAN_POINT('Ctrl Pts',(88.3508939033027,1.46818633188394,3.33398052643478));
#8009=CARTESIAN_POINT('Ctrl Pts',(88.2950641342964,2.54306224328792,2.60841555020236));
#8010=CARTESIAN_POINT('Ctrl Pts',(88.23923436529,3.06926334215677,1.59730874281291));
#8011=CARTESIAN_POINT('Ctrl Pts',(88.1834045962837,3.59546444102562,0.586201935423477));
#8012=CARTESIAN_POINT('Ctrl Pts',(88.1275748272773,3.57299072735933,-0.710446703122968));
#8013=CARTESIAN_POINT('Ctrl Pts',(88.0717450582709,3.01206688724067,-1.70271129383767));
#8014=CARTESIAN_POINT('Ctrl Pts',(88.0159152892645,2.45114304712202,-2.69497588455235));
#8015=CARTESIAN_POINT('Ctrl Pts',(87.9600855202581,1.35176908055096,-3.38285642743532));
#8016=CARTESIAN_POINT('Ctrl Pts',(87.9042557512518,0.214118383995447,-3.45339340374213));
#8017=CARTESIAN_POINT('Ctrl Pts',(87.8484259822454,-0.923532312560085,-3.52393038004894));
#8018=CARTESIAN_POINT('Ctrl Pts',(87.7925962132391,-2.0994597391001,-2.97712378977962));
#8019=CARTESIAN_POINT('Ctrl Pts',(87.7367664442328,-2.77866158265664,-2.06174986175392));
#8020=CARTESIAN_POINT('Ctrl Pts',(87.7009250172118,-3.21469353732137,-1.47410086334105));
#8021=CARTESIAN_POINT('Ctrl Pts',(87.6650835901909,-3.446007764652,-0.734552566120437));
#8022=CARTESIAN_POINT('Ctrl Pts',(87.6292421631699,-3.45063882513586,0.00234158759808215));
#8023=CARTESIAN_POINT('Origin',(84.65,0.,0.));
#8024=CARTESIAN_POINT('',(86.5709088298366,-3.45978675425269,0.000812295043242979));
#8025=CARTESIAN_POINT('',(86.868373286472,-3.44956363082089,-0.00156881125221945));
#8026=CARTESIAN_POINT('',(84.65,-3.4544,-4.23041990297462E-16));
#8027=CARTESIAN_POINT('Ctrl Pts',(86.868373286472,-3.44956363082089,-0.00156881125221945));
#8028=CARTESIAN_POINT('Ctrl Pts',(86.8913616617206,-3.45151572191023,-0.474576012219106));
#8029=CARTESIAN_POINT('Ctrl Pts',(86.9143500369692,-3.3608767438491,-0.946867197435236));
#8030=CARTESIAN_POINT('Ctrl Pts',(86.9373384122178,-3.17403716751804,-1.37741099447087));
#8031=CARTESIAN_POINT('Ctrl Pts',(86.9931681812242,-2.7202769397939,-2.42303342214078));
#8032=CARTESIAN_POINT('Ctrl Pts',(87.0489979502306,-1.69911207658363,-3.22242389284734));
#8033=CARTESIAN_POINT('Ctrl Pts',(87.1048277192369,-0.575133802999295,-3.41189010624943));
#8034=CARTESIAN_POINT('Ctrl Pts',(87.1606574882433,0.548844470585059,-3.60135631965152));
#8035=CARTESIAN_POINT('Ctrl Pts',(87.2164872572496,1.77563615454348,-3.18089827574911));
#8036=CARTESIAN_POINT('Ctrl Pts',(87.272317026256,2.54709763079675,-2.34180841395378));
#8037=CARTESIAN_POINT('Ctrl Pts',(87.3281467952623,3.31855910705,-1.50271855215846));
#8038=CARTESIAN_POINT('Ctrl Pts',(87.3839765642687,3.6346903755981,-0.244996872470229));
#8039=CARTESIAN_POINT('Ctrl Pts',(87.4398063332751,3.35166371709586,0.859141033811245));
#8040=CARTESIAN_POINT('Ctrl Pts',(87.4956361022814,3.06863705859362,1.96327894009272));
#8041=CARTESIAN_POINT('Ctrl Pts',(87.5514658712878,2.18645247304104,2.91383307296744));
#8042=CARTESIAN_POINT('Ctrl Pts',(87.6072956402942,1.106470438205,3.27833740756711));
#8043=CARTESIAN_POINT('Ctrl Pts',(87.6631254093005,0.026488403368936,3.64284174216678));
#8044=CARTESIAN_POINT('Ctrl Pts',(87.7189551783069,-1.25129108075059,3.4212962784914));
#8045=CARTESIAN_POINT('Ctrl Pts',(87.7747849473132,-2.14552688370774,2.71449578739078));
#8046=CARTESIAN_POINT('Ctrl Pts',(87.8254255048106,-2.95664611994735,2.07339030646564));
#8047=CARTESIAN_POINT('Ctrl Pts',(87.876066062308,-3.45220667922921,1.03304363878092));
#8048=CARTESIAN_POINT('Ctrl Pts',(87.9267066198054,-3.45881529047273,-0.00181033228093454));
#8049=CARTESIAN_POINT('Ctrl Pts',(87.6292421631699,-3.45063882513586,0.00234158759808215));
#8050=CARTESIAN_POINT('Ctrl Pts',(87.6092538211845,-3.45322151305876,0.413298783665407));
#8051=CARTESIAN_POINT('Ctrl Pts',(87.5892654791991,-3.38530207254061,0.823430498208507));
#8052=CARTESIAN_POINT('Ctrl Pts',(87.5692771372136,-3.24307059694375,1.20592942853766));
#8053=CARTESIAN_POINT('Ctrl Pts',(87.5134473682073,-2.84580150710126,2.27429352502138));
#8054=CARTESIAN_POINT('Ctrl Pts',(87.457617599201,-1.86878706684323,3.12708045220674));
#8055=CARTESIAN_POINT('Ctrl Pts',(87.4017878301946,-0.756531735836134,3.37630455025122));
#8056=CARTESIAN_POINT('Ctrl Pts',(87.3459580611882,0.355723595170976,3.62552864829569));
#8057=CARTESIAN_POINT('Ctrl Pts',(87.2901282921818,1.60321981692717,3.27118991719926));
#8058=CARTESIAN_POINT('Ctrl Pts',(87.2342985231755,2.41839353309076,2.47449902050477));
#8059=CARTESIAN_POINT('Ctrl Pts',(87.1784687541691,3.23356724925433,1.67780812381029));
#8060=CARTESIAN_POINT('Ctrl Pts',(87.1226389851628,3.61641845982532,0.438765061517766));
#8061=CARTESIAN_POINT('Ctrl Pts',(87.0668092161565,3.39276440611025,-0.678912636504609));
#8062=CARTESIAN_POINT('Ctrl Pts',(87.0109794471501,3.16911035239517,-1.796590334527));
#8063=CARTESIAN_POINT('Ctrl Pts',(86.9551496781437,2.33895103439404,-2.79290266827921));
#8064=CARTESIAN_POINT('Ctrl Pts',(86.8993199091373,1.27997740925145,-3.2145653695609));
#8065=CARTESIAN_POINT('Ctrl Pts',(86.843490140131,0.221003784108877,-3.63622807084259));
#8066=CARTESIAN_POINT('Ctrl Pts',(86.7876603711246,-1.06678414817515,-3.48324113965374));
#8067=CARTESIAN_POINT('Ctrl Pts',(86.7318306021183,-1.99749179339816,-2.82520781867127));
#8068=CARTESIAN_POINT('Ctrl Pts',(86.6781900113577,-2.89170484144875,-2.19297708037795));
#8069=CARTESIAN_POINT('Ctrl Pts',(86.6245494205971,-3.4562919977347,-1.09453083635498));
#8070=CARTESIAN_POINT('Ctrl Pts',(86.5709088298366,-3.45978675425269,0.00081229504324298));
#8071=CARTESIAN_POINT('Origin',(84.65,0.,0.));
#8072=CARTESIAN_POINT('',(85.5125754965032,-3.45287610787495,-0.00301865808173374));
#8073=CARTESIAN_POINT('',(85.8100399531387,-3.45320716154862,0.00305860587857352));
#8074=CARTESIAN_POINT('',(84.65,-3.4544,-4.23041990297462E-16));
#8075=CARTESIAN_POINT('Ctrl Pts',(85.8100399531387,-3.45320716154862,0.00305860587857352));
#8076=CARTESIAN_POINT('Ctrl Pts',(85.8508274921269,-3.44594376666017,-0.833950371543459));
#8077=CARTESIAN_POINT('Ctrl Pts',(85.8916150311151,-3.13961127392647,-1.67572430432957));
#8078=CARTESIAN_POINT('Ctrl Pts',(85.9324025701033,-2.58649539295724,-2.29821986996156));
#8079=CARTESIAN_POINT('Ctrl Pts',(85.9882323391097,-1.82939328201139,-3.15028852864581));
#8080=CARTESIAN_POINT('Ctrl Pts',(86.0440621081161,-0.609918048706947,-3.5915174464072));
#8081=CARTESIAN_POINT('Ctrl Pts',(86.0998918771225,0.517115396018346,-3.42116422518358));
#8082=CARTESIAN_POINT('Ctrl Pts',(86.1557216461288,1.64414884074359,-3.25081100395996));
#8083=CARTESIAN_POINT('Ctrl Pts',(86.2115514151351,2.67874049688969,-2.46887564375138));
#8084=CARTESIAN_POINT('Ctrl Pts',(86.2673811841415,3.15019045855844,-1.43110903263256));
#8085=CARTESIAN_POINT('Ctrl Pts',(86.3232109531478,3.62164042022721,-0.393342421513706));
#8086=CARTESIAN_POINT('Ctrl Pts',(86.3790407221543,3.52994868741858,0.900255440515412));
#8087=CARTESIAN_POINT('Ctrl Pts',(86.4348704911606,2.91683151576663,1.86114666190112));
#8088=CARTESIAN_POINT('Ctrl Pts',(86.490700260167,2.3037143441147,2.82203788328681));
#8089=CARTESIAN_POINT('Ctrl Pts',(86.5465300291733,1.16917173361946,3.45022246402909));
#8090=CARTESIAN_POINT('Ctrl Pts',(86.6023597981796,0.0293774778981162,3.4599002806826));
#8091=CARTESIAN_POINT('Ctrl Pts',(86.658189567186,-1.11041677782324,3.4695780973361));
#8092=CARTESIAN_POINT('Ctrl Pts',(86.7140193361924,-2.25546267877071,2.8607491499008));
#8093=CARTESIAN_POINT('Ctrl Pts',(86.7698491051988,-2.88480783312544,1.91040748386653));
#8094=CARTESIAN_POINT('Ctrl Pts',(86.8026904989565,-3.25501484618601,1.35137696280011));
#8095=CARTESIAN_POINT('Ctrl Pts',(86.8355318927143,-3.44677485643284,0.67417340929306));
#8096=CARTESIAN_POINT('Ctrl Pts',(86.868373286472,-3.44956363082089,-0.00156881125221945));
#8097=CARTESIAN_POINT('Ctrl Pts',(86.5709088298366,-3.45978675425269,0.00081229504324298));
#8098=CARTESIAN_POINT('Ctrl Pts',(86.5687196515908,-3.45992938215508,0.0455154073866809));
#8099=CARTESIAN_POINT('Ctrl Pts',(86.566530473345,-3.45913744502121,0.0902133511329964));
#8100=CARTESIAN_POINT('Ctrl Pts',(86.5643412950992,-3.45739520842613,0.134874223357528));
#8101=CARTESIAN_POINT('Ctrl Pts',(86.5085115260929,-3.41296362006907,1.27384323362772));
#8102=CARTESIAN_POINT('Ctrl Pts',(86.4526817570865,-2.75047308519294,2.388701543392));
#8103=CARTESIAN_POINT('Ctrl Pts',(86.3968519880802,-1.77133163330598,2.97223096818263));
#8104=CARTESIAN_POINT('Ctrl Pts',(86.3410222190738,-0.792190181419031,3.55576039297326));
#8105=CARTESIAN_POINT('Ctrl Pts',(86.2851924500674,0.503602187478725,3.60796093279025));
#8106=CARTESIAN_POINT('Ctrl Pts',(86.229362681061,1.52650916456398,3.10508332478799));
#8107=CARTESIAN_POINT('Ctrl Pts',(86.1735329120547,2.54941614164925,2.60220571678573));
#8108=CARTESIAN_POINT('Ctrl Pts',(86.1177031430483,3.299437726922,1.54424996096417));
#8109=CARTESIAN_POINT('Ctrl Pts',(86.061873374042,3.43534258769914,0.412545741118299));
#8110=CARTESIAN_POINT('Ctrl Pts',(86.0060436050356,3.57124744847628,-0.719158478727583));
#8111=CARTESIAN_POINT('Ctrl Pts',(85.9502138360292,3.09303558475781,-1.92461116259779));
#8112=CARTESIAN_POINT('Ctrl Pts',(85.8943840670229,2.21827523026619,-2.65537712691846));
#8113=CARTESIAN_POINT('Ctrl Pts',(85.8385542980165,1.34351487577459,-3.38614309123912));
#8114=CARTESIAN_POINT('Ctrl Pts',(85.7827245290102,0.072206030509842,-3.64222233601026));
#8115=CARTESIAN_POINT('Ctrl Pts',(85.7268947600038,-1.0172540699822,-3.30710853170544));
#8116=CARTESIAN_POINT('Ctrl Pts',(85.6710649909975,-2.10671417047426,-2.97199472740061));
#8117=CARTESIAN_POINT('Ctrl Pts',(85.6152352219911,-3.01432552619362,-2.04568787401981));
#8118=CARTESIAN_POINT('Ctrl Pts',(85.5594054529847,-3.32715944475099,-0.949622405263555));
#8119=CARTESIAN_POINT('Ctrl Pts',(85.5437954674909,-3.41462770796557,-0.643162852016612));
#8120=CARTESIAN_POINT('Ctrl Pts',(85.528185481997,-3.4555986618466,-0.323432252563192));
#8121=CARTESIAN_POINT('Ctrl Pts',(85.5125754965032,-3.45287610787495,-0.00301865808173374));
#8122=CARTESIAN_POINT('Origin',(84.65,0.,0.));
#8123=CARTESIAN_POINT('',(84.4542421631699,-3.44973260108164,0.00172992572337771));
#8124=CARTESIAN_POINT('',(84.7517066198054,-3.45965414368361,-0.0010147492130462));
#8125=CARTESIAN_POINT('',(84.65,-3.4544,-4.23041990297462E-16));
#8126=CARTESIAN_POINT('Ctrl Pts',(84.7517066198054,-3.45965414368361,-0.0010147492130462));
#8127=CARTESIAN_POINT('Ctrl Pts',(84.7544635535269,-3.45987358617366,-0.0573172245063646));
#8128=CARTESIAN_POINT('Ctrl Pts',(84.7572204872483,-3.45861734950704,-0.11360970225368));
#8129=CARTESIAN_POINT('Ctrl Pts',(84.7599774209698,-3.45585465379575,-0.169828149355248));
#8130=CARTESIAN_POINT('Ctrl Pts',(84.8158071899762,-3.39990820060586,-1.30828965502245));
#8131=CARTESIAN_POINT('Ctrl Pts',(84.8716369589825,-2.72617819711704,-2.41639194493554));
#8132=CARTESIAN_POINT('Ctrl Pts',(84.9274667279889,-1.74118620413938,-2.98999056704028));
#8133=CARTESIAN_POINT('Ctrl Pts',(84.9832964969953,-0.756194211161706,-3.56358918914502));
#8134=CARTESIAN_POINT('Ctrl Pts',(85.0391262660017,0.540059771304828,-3.60268414344138));
#8135=CARTESIAN_POINT('Ctrl Pts',(85.094956035008,1.55782941779685,-3.08948871069662));
#8136=CARTESIAN_POINT('Ctrl Pts',(85.1507858040143,2.57559906428888,-2.57629327795187));
#8137=CARTESIAN_POINT('Ctrl Pts',(85.2066155730207,3.31488437480642,-1.510807458166));
#8138=CARTESIAN_POINT('Ctrl Pts',(85.262445342027,3.43933861387626,-0.377786828217834));
#8139=CARTESIAN_POINT('Ctrl Pts',(85.3182751110334,3.56379285294609,0.7552338017303));
#8140=CARTESIAN_POINT('Ctrl Pts',(85.3741048800397,3.07341602056828,1.95578924184072));
#8141=CARTESIAN_POINT('Ctrl Pts',(85.4299346490461,2.1913109491344,2.67767236843473));
#8142=CARTESIAN_POINT('Ctrl Pts',(85.4857644180525,1.30920587770051,3.39955549502874));
#8143=CARTESIAN_POINT('Ctrl Pts',(85.5415941870588,0.0353725672105228,3.64276630810633));
#8144=CARTESIAN_POINT('Ctrl Pts',(85.5974239560652,-1.05064321100081,3.2966531257706));
#8145=CARTESIAN_POINT('Ctrl Pts',(85.6532537250716,-2.13665898921217,2.95053994343486));
#8146=CARTESIAN_POINT('Ctrl Pts',(85.7090834940779,-3.03485723514488,2.01510276568579));
#8147=CARTESIAN_POINT('Ctrl Pts',(85.7649132630843,-3.3365918638176,0.915929977007713));
#8148=CARTESIAN_POINT('Ctrl Pts',(85.7799554931024,-3.41788830780643,0.619779550250641));
#8149=CARTESIAN_POINT('Ctrl Pts',(85.7949977231206,-3.45588586341039,0.311743117814283));
#8150=CARTESIAN_POINT('Ctrl Pts',(85.8100399531387,-3.45320716154862,0.00305860587857352));
#8151=CARTESIAN_POINT('Ctrl Pts',(85.5125754965032,-3.45287610787495,-0.00301865808173374));
#8152=CARTESIAN_POINT('Ctrl Pts',(85.4723557129907,-3.44586133317295,0.822540430977856));
#8153=CARTESIAN_POINT('Ctrl Pts',(85.4321359294782,-3.14878420194866,1.65263362949813));
#8154=CARTESIAN_POINT('Ctrl Pts',(85.3919161459656,-2.60960248063633,2.2719479695695));
#8155=CARTESIAN_POINT('Ctrl Pts',(85.3360863769593,-1.86115511656889,3.13162879151465));
#8156=CARTESIAN_POINT('Ctrl Pts',(85.2802566079529,-0.6462039070386,3.58516635127327));
#8157=CARTESIAN_POINT('Ctrl Pts',(85.2244268389466,0.482494495994766,3.42621828620259));
#8158=CARTESIAN_POINT('Ctrl Pts',(85.1685970699402,1.61119289902813,3.26727022113191));
#8159=CARTESIAN_POINT('Ctrl Pts',(85.1127673009339,2.65363849556458,2.49583653123193));
#8160=CARTESIAN_POINT('Ctrl Pts',(85.0569375319275,3.13555813515021,1.46289024347954));
#8161=CARTESIAN_POINT('Ctrl Pts',(85.0011077629212,3.61747777473585,0.42994395572713));
#8162=CARTESIAN_POINT('Ctrl Pts',(84.9452779939148,3.53887145737065,-0.864514929877678));
#8163=CARTESIAN_POINT('Ctrl Pts',(84.8894482249084,2.9355020716948,-1.83155678875917));
#8164=CARTESIAN_POINT('Ctrl Pts',(84.833618455902,2.33213268601896,-2.79859864764063));
#8165=CARTESIAN_POINT('Ctrl Pts',(84.7777886868957,1.2040002320325,-3.43822347979879));
#8166=CARTESIAN_POINT('Ctrl Pts',(84.7219589178894,0.0643621256227443,-3.45942628193745));
#8167=CARTESIAN_POINT('Ctrl Pts',(84.666129148883,-1.07527598078704,-3.48062908407612));
#8168=CARTESIAN_POINT('Ctrl Pts',(84.6102993798766,-2.22641973962013,-2.88340985619525));
#8169=CARTESIAN_POINT('Ctrl Pts',(84.5544696108703,-2.86534246533909,-1.93948066236783));
#8170=CARTESIAN_POINT('Ctrl Pts',(84.5210604616368,-3.24768086780961,-1.37462302702994));
#8171=CARTESIAN_POINT('Ctrl Pts',(84.4876513124034,-3.44659509347488,-0.685610025194725));
#8172=CARTESIAN_POINT('Ctrl Pts',(84.4542421631699,-3.44973260108164,0.00172992572337771));
#8173=CARTESIAN_POINT('Origin',(84.65,0.,0.));
#8174=CARTESIAN_POINT('',(83.3959088298365,-3.45904630125211,0.00163698504970649));
#8175=CARTESIAN_POINT('',(83.6933732864721,-3.45040227751753,-0.00221153198392862));
#8176=CARTESIAN_POINT('',(84.65,-3.4544,-4.23041990297462E-16));
#8177=CARTESIAN_POINT('Ctrl Pts',(83.6933732864721,-3.45040227751753,-0.00221153198392862));
#8178=CARTESIAN_POINT('Ctrl Pts',(83.7139293839331,-3.45289985741792,-0.424914548013618));
#8179=CARTESIAN_POINT('Ctrl Pts',(83.7344854813943,-3.38095223892544,-0.84679701239954));
#8180=CARTESIAN_POINT('Ctrl Pts',(83.7550415788554,-3.23071059867279,-1.23866138072456));
#8181=CARTESIAN_POINT('Ctrl Pts',(83.8108713478617,-2.82265862838445,-2.30295372545619));
#8182=CARTESIAN_POINT('Ctrl Pts',(83.866701116868,-1.8370708345208,-3.1458175953063));
#8183=CARTESIAN_POINT('Ctrl Pts',(83.9225308858744,-0.722352226990953,-3.38378194460523));
#8184=CARTESIAN_POINT('Ctrl Pts',(83.9783606548808,0.392366380538912,-3.62174629390416));
#8185=CARTESIAN_POINT('Ctrl Pts',(84.0341904238871,1.636215801735,-3.25481112265189));
#8186=CARTESIAN_POINT('Ctrl Pts',(84.0900201928935,2.44329179599138,-2.44991799620239));
#8187=CARTESIAN_POINT('Ctrl Pts',(84.1458499618999,3.25036779024777,-1.6450248697529));
#8188=CARTESIAN_POINT('Ctrl Pts',(84.2016797309063,3.62067035756447,-0.402173788106215));
#8189=CARTESIAN_POINT('Ctrl Pts',(84.2575094999126,3.38572589528446,0.713185214706118));
#8190=CARTESIAN_POINT('Ctrl Pts',(84.313339268919,3.15078143300445,1.82854421751844));
#8191=CARTESIAN_POINT('Ctrl Pts',(84.3691690379253,2.31058994112772,2.8164111414964));
#8192=CARTESIAN_POINT('Ctrl Pts',(84.4249988069317,1.24740663485295,3.22734405909875));
#8193=CARTESIAN_POINT('Ctrl Pts',(84.480828575938,0.184223328578151,3.6382769767011));
#8194=CARTESIAN_POINT('Ctrl Pts',(84.5366583449444,-1.10195179209471,3.47227588792783));
#8195=CARTESIAN_POINT('Ctrl Pts',(84.5924881139508,-2.02595790098566,2.80486498283053));
#8196=CARTESIAN_POINT('Ctrl Pts',(84.6455609492356,-2.90433559969705,2.17041154223815));
#8197=CARTESIAN_POINT('Ctrl Pts',(84.6986337845205,-3.45542972760911,1.08284590876941));
#8198=CARTESIAN_POINT('Ctrl Pts',(84.7517066198054,-3.45965414368361,-0.0010147492130462));
#8199=CARTESIAN_POINT('Ctrl Pts',(84.4542421631699,-3.44973260108164,0.00172992572337771));
#8200=CARTESIAN_POINT('Ctrl Pts',(84.431821543397,-3.45183815799343,0.462998411986782));
#8201=CARTESIAN_POINT('Ctrl Pts',(84.4094009236241,-3.36577278153509,0.923513415086305));
#8202=CARTESIAN_POINT('Ctrl Pts',(84.3869803038512,-3.18780308562104,1.34524502254394));
#8203=CARTESIAN_POINT('Ctrl Pts',(84.3311505348448,-2.74463928757921,2.39540235385431));
#8204=CARTESIAN_POINT('Ctrl Pts',(84.2753207658384,-1.73160999889071,3.20507785670111));
#8205=CARTESIAN_POINT('Ctrl Pts',(84.2194909968321,-0.609605067279678,3.40589993178326));
#8206=CARTESIAN_POINT('Ctrl Pts',(84.1636612278257,0.512399864331356,3.60672200686541));
#8207=CARTESIAN_POINT('Ctrl Pts',(84.1078314588194,1.74338043886494,3.19869065418292));
#8208=CARTESIAN_POINT('Ctrl Pts',(84.052001689813,2.52328725213983,2.36744464065433));
#8209=CARTESIAN_POINT('Ctrl Pts',(83.9961719208067,3.30319406541474,1.53619862712572));
#8210=CARTESIAN_POINT('Ctrl Pts',(83.9403421518003,3.63202711743095,0.281737952751017));
#8211=CARTESIAN_POINT('Ctrl Pts',(83.8845123827939,3.36017985982636,-0.825205424722592));
#8212=CARTESIAN_POINT('Ctrl Pts',(83.8286826137876,3.08833260222177,-1.93214880219619));
#8213=CARTESIAN_POINT('Ctrl Pts',(83.7728528447812,2.21580503499638,-2.89157488276869));
#8214=CARTESIAN_POINT('Ctrl Pts',(83.7170230757749,1.1395640593878,-3.26698124235905));
#8215=CARTESIAN_POINT('Ctrl Pts',(83.6611933067685,0.0633230837792188,-3.64238760194941));
#8216=CARTESIAN_POINT('Ctrl Pts',(83.6053635377622,-1.21663130021256,-3.43377424055763));
#8217=CARTESIAN_POINT('Ctrl Pts',(83.5495337687558,-2.11796846531068,-2.73605231370378));
#8218=CARTESIAN_POINT('Ctrl Pts',(83.4983254557827,-2.94469507489686,-2.09608615524738));
#8219=CARTESIAN_POINT('Ctrl Pts',(83.4471171428096,-3.45289220190666,-1.04463448977794));
#8220=CARTESIAN_POINT('Ctrl Pts',(83.3959088298365,-3.45904630125211,0.00163698504970649));
#8221=CARTESIAN_POINT('Origin',(84.65,0.,0.));
#8222=CARTESIAN_POINT('',(82.3375754965033,-3.45433093919597,-0.00310444462076481));
#8223=CARTESIAN_POINT('',(82.6350399531387,-3.4518452061196,0.00280651627479178));
#8224=CARTESIAN_POINT('',(84.65,-3.4544,-4.23041990297462E-16));
#8225=CARTESIAN_POINT('Ctrl Pts',(82.6350399531387,-3.4518452061196,0.00280651627479178));
#8226=CARTESIAN_POINT('Ctrl Pts',(82.6733952143394,-3.44576312325575,-0.785076990999158));
#8227=CARTESIAN_POINT('Ctrl Pts',(82.7117504755402,-3.17789065414655,-1.57670048768815));
#8228=CARTESIAN_POINT('Ctrl Pts',(82.7501057367409,-2.68359731851267,-2.18405091986124));
#8229=CARTESIAN_POINT('Ctrl Pts',(82.8059355057472,-1.9641058619064,-3.06810784641131));
#8230=CARTESIAN_POINT('Ctrl Pts',(82.8617652747536,-0.764882922038081,-3.56173436819202));
#8231=CARTESIAN_POINT('Ctrl Pts',(82.9175950437599,0.368470614410377,-3.44034916756878));
#8232=CARTESIAN_POINT('Ctrl Pts',(82.9734248127663,1.50182415085883,-3.31896396694554));
#8233=CARTESIAN_POINT('Ctrl Pts',(83.0292545817727,2.56930828388742,-2.58256704391836));
#8234=CARTESIAN_POINT('Ctrl Pts',(83.085084350779,3.0852582799953,-1.56619102736403));
#8235=CARTESIAN_POINT('Ctrl Pts',(83.1409141197854,3.60120827610318,-0.549815010809704));
#8236=CARTESIAN_POINT('Ctrl Pts',(83.1967438887917,3.56562413529035,0.746540099271768));
#8237=CARTESIAN_POINT('Ctrl Pts',(83.2525736577981,2.9946952900083,1.73308196819345));
#8238=CARTESIAN_POINT('Ctrl Pts',(83.3084034268044,2.42376644472625,2.71962383711512));
#8239=CARTESIAN_POINT('Ctrl Pts',(83.3642331958109,1.31749289497499,3.39635246487701));
#8240=CARTESIAN_POINT('Ctrl Pts',(83.4200629648172,0.179187085497533,3.45538203052369));
#8241=CARTESIAN_POINT('Ctrl Pts',(83.4758927338236,-0.959118723979919,3.51441159617038));
#8242=CARTESIAN_POINT('Ctrl Pts',(83.5317225028299,-2.12945679318357,2.95574209970188));
#8243=CARTESIAN_POINT('Ctrl Pts',(83.5875522718362,-2.79936775442887,2.03354694166105));
#8244=CARTESIAN_POINT('Ctrl Pts',(83.6228259433815,-3.22262258123717,1.45089704565928));
#8245=CARTESIAN_POINT('Ctrl Pts',(83.6580996149268,-3.44611650230016,0.723134676207329));
#8246=CARTESIAN_POINT('Ctrl Pts',(83.6933732864721,-3.45040227751753,-0.00221153198392862));
#8247=CARTESIAN_POINT('Ctrl Pts',(83.3959088298365,-3.45904630125211,0.00163698504970649));
#8248=CARTESIAN_POINT('Ctrl Pts',(83.3912873738032,-3.45960169739579,0.096061060733295));
#8249=CARTESIAN_POINT('Ctrl Pts',(83.38666591777,-3.45606808841924,0.190442945160575));
#8250=CARTESIAN_POINT('Ctrl Pts',(83.3820444617367,-3.44831058325344,0.284476369487177));
#8251=CARTESIAN_POINT('Ctrl Pts',(83.3262146927303,-3.35459558989358,1.42045263350827));
#8252=CARTESIAN_POINT('Ctrl Pts',(83.2703849237241,-2.64444565696942,2.50557466923451));
#8253=CARTESIAN_POINT('Ctrl Pts',(83.2145551547177,-1.6409520298194,3.04615316739094));
#8254=CARTESIAN_POINT('Ctrl Pts',(83.1587253857113,-0.637458402669365,3.58673166554739));
#8255=CARTESIAN_POINT('Ctrl Pts',(83.1028956167049,0.659378918706555,3.58276662613398));
#8256=CARTESIAN_POINT('Ctrl Pts',(83.0470658476985,1.65954821179859,3.03606199147685));
#8257=CARTESIAN_POINT('Ctrl Pts',(82.9912360786921,2.65971750489062,2.48935735681972));
#8258=CARTESIAN_POINT('Ctrl Pts',(82.9354063096858,3.36321876969879,1.39991312691889));
#8259=CARTESIAN_POINT('Ctrl Pts',(82.8795765406795,3.44998565233621,0.263385045225713));
#8260=CARTESIAN_POINT('Ctrl Pts',(82.8237467716731,3.53675253497364,-0.873143036467469));
#8261=CARTESIAN_POINT('Ctrl Pts',(82.7679170026668,3.0067850354403,-2.05675496995299));
#8262=CARTESIAN_POINT('Ctrl Pts',(82.7120872336604,2.10119823588243,-2.7489522834889));
#8263=CARTESIAN_POINT('Ctrl Pts',(82.656257464654,1.19561143632454,-3.44114959702482));
#8264=CARTESIAN_POINT('Ctrl Pts',(82.6004276956476,-0.0855946632578827,
-3.64193229061111));
#8265=CARTESIAN_POINT('Ctrl Pts',(82.5445979266412,-1.15951995253908,-3.25995186514127));
#8266=CARTESIAN_POINT('Ctrl Pts',(82.4887681576349,-2.23344524182026,-2.87797143967144));
#8267=CARTESIAN_POINT('Ctrl Pts',(82.4329383886286,-3.10008972080022,-1.91322789514549));
#8268=CARTESIAN_POINT('Ctrl Pts',(82.3771086196223,-3.36516306993141,-0.804642899766173));
#8269=CARTESIAN_POINT('Ctrl Pts',(82.3639309119159,-3.42772931689531,-0.542979466498652));
#8270=CARTESIAN_POINT('Ctrl Pts',(82.3507532042096,-3.45678088484327,-0.273302350699935));
#8271=CARTESIAN_POINT('Ctrl Pts',(82.3375754965033,-3.45433093919597,-0.00310444462076481));
#8272=CARTESIAN_POINT('Origin',(84.65,0.,0.));
#8273=CARTESIAN_POINT('',(81.2792421631699,-3.44913158907647,0.00100292261883378));
#8274=CARTESIAN_POINT('',(81.5767066198053,-3.46001944289485,-0.000122141770493717));
#8275=CARTESIAN_POINT('',(84.65,-3.4544,-4.23041990297462E-16));
#8276=CARTESIAN_POINT('Ctrl Pts',(81.5767066198053,-3.46001944289485,-0.000122141770493717));
#8277=CARTESIAN_POINT('Ctrl Pts',(81.5770312757393,-3.46002289260932,-0.00675043203261977));
#8278=CARTESIAN_POINT('Ctrl Pts',(81.5773559316733,-3.4600054815873,-0.013378703645769));
#8279=CARTESIAN_POINT('Ctrl Pts',(81.5776805876073,-3.45996715508333,-0.0200068543175971));
#8280=CARTESIAN_POINT('Ctrl Pts',(81.6335103566137,-3.45337630107705,-1.15982314045938));
#8281=CARTESIAN_POINT('Ctrl Pts',(81.68934012562,-2.82826672822439,-2.29606291464425));
#8282=CARTESIAN_POINT('Ctrl Pts',(81.7451698946264,-1.86903954818118,-2.91178023824083));
#8283=CARTESIAN_POINT('Ctrl Pts',(81.8009996636328,-0.909812368137995,-3.52749756183741));
#8284=CARTESIAN_POINT('Ctrl Pts',(81.8568294326391,0.383532419095744,-3.6226924348457));
#8285=CARTESIAN_POINT('Ctrl Pts',(81.9126592016455,1.42257206138549,-3.15405480590312));
#8286=CARTESIAN_POINT('Ctrl Pts',(81.9684889706519,2.46161170367527,-2.68541717696053));
#8287=CARTESIAN_POINT('Ctrl Pts',(82.0243187396582,3.24634620102107,-1.65294704606706));
#8288=CARTESIAN_POINT('Ctrl Pts',(82.0801485086645,3.4197511642724,-0.526379105714418));
#8289=CARTESIAN_POINT('Ctrl Pts',(82.1359782776709,3.59315612752373,0.600188834638211));
#8290=CARTESIAN_POINT('Ctrl Pts',(82.1918080466773,3.15523155668061,1.82085458444999));
#8291=CARTESIAN_POINT('Ctrl Pts',(82.2476378156836,2.30521649746879,2.58026159299263));
#8292=CARTESIAN_POINT('Ctrl Pts',(82.30346758469,1.45520143825698,3.33966860153526));
#8293=CARTESIAN_POINT('Ctrl Pts',(82.3592973536963,0.193095890676444,3.63781686880876));
#8294=CARTESIAN_POINT('Ctrl Pts',(82.4151271227027,-0.906890060597697,3.33906025798641));
#8295=CARTESIAN_POINT('Ctrl Pts',(82.4709568917091,-2.00687601187186,3.04030364716405));
#8296=CARTESIAN_POINT('Ctrl Pts',(82.5267866607154,-2.94474236683964,2.14464215824585));
#8297=CARTESIAN_POINT('Ctrl Pts',(82.5826164297218,-3.29379555765141,1.05956774812703));
#8298=CARTESIAN_POINT('Ctrl Pts',(82.6000909375274,-3.40304789410166,0.719943537123092));
#8299=CARTESIAN_POINT('Ctrl Pts',(82.617565445333,-3.45461617941379,0.361763177415482));
#8300=CARTESIAN_POINT('Ctrl Pts',(82.6350399531387,-3.4518452061196,0.00280651627479178));
#8301=CARTESIAN_POINT('Ctrl Pts',(82.3375754965033,-3.45433093919597,-0.00310444462076481));
#8302=CARTESIAN_POINT('Ctrl Pts',(82.2949234352032,-3.44640124199378,0.871440499769488));
#8303=CARTESIAN_POINT('Ctrl Pts',(82.2522713739032,-3.10845802640836,1.75144130367814));
#8304=CARTESIAN_POINT('Ctrl Pts',(82.2096193126031,-2.50876343656488,2.38282997772174));
#8305=CARTESIAN_POINT('Ctrl Pts',(82.1537895435968,-1.72378823478477,3.20929141359766));
#8306=CARTESIAN_POINT('Ctrl Pts',(82.0979597745904,-0.490335611942143,3.60978783911679));
#8307=CARTESIAN_POINT('Ctrl Pts',(82.0421300055841,0.630420339698764,3.40210859301528));
#8308=CARTESIAN_POINT('Ctrl Pts',(81.9863002365777,1.75117629133966,3.19442934691377));
#8309=CARTESIAN_POINT('Ctrl Pts',(81.9304704675714,2.75923557177884,2.37857442919163));
#8310=CARTESIAN_POINT('Ctrl Pts',(81.874640698565,3.19596949826618,1.32572683820102));
#8311=CARTESIAN_POINT('Ctrl Pts',(81.8188109295586,3.63270342475352,0.272879247210409));
#8312=CARTESIAN_POINT('Ctrl Pts',(81.7629811605522,3.49811199728901,-1.01696101704867));
#8313=CARTESIAN_POINT('Ctrl Pts',(81.7071513915459,2.85342920308481,-1.9569656272804));
#8314=CARTESIAN_POINT('Ctrl Pts',(81.6513216225396,2.20874640888062,-2.89697023751212));
#8315=CARTESIAN_POINT('Ctrl Pts',(81.5954918535332,1.05397224793672,-3.4871391937165));
#8316=CARTESIAN_POINT('Ctrl Pts',(81.5396620845269,-0.0855148991452379,
-3.45896803763762));
#8317=CARTESIAN_POINT('Ctrl Pts',(81.4838323155205,-1.22500204622719,-3.43079688155875));
#8318=CARTESIAN_POINT('Ctrl Pts',(81.4280025465141,-2.34920217944721,-2.78428561319665));
#8319=CARTESIAN_POINT('Ctrl Pts',(81.3721727775078,-2.94664693950248,-1.81357230274801));
#8320=CARTESIAN_POINT('Ctrl Pts',(81.3411959060618,-3.27813621229857,-1.27497681930224));
#8321=CARTESIAN_POINT('Ctrl Pts',(81.3102190346159,-3.44746224273321,-0.636574751997453));
#8322=CARTESIAN_POINT('Ctrl Pts',(81.2792421631699,-3.44913158907647,0.00100292261883378));
#8323=CARTESIAN_POINT('Origin',(84.65,0.,0.));
#8324=CARTESIAN_POINT('',(80.2209088298365,-3.45793510972046,0.00231429949518289));
#8325=CARTESIAN_POINT('',(80.5183732864721,-3.45151093143175,-0.00270500195080525));
#8326=CARTESIAN_POINT('',(84.65,-3.4544,-4.23041990297462E-16));
#8327=CARTESIAN_POINT('Ctrl Pts',(80.5183732864721,-3.45151093143175,-0.00270500195080525));
#8328=CARTESIAN_POINT('Ctrl Pts',(80.5364971061457,-3.45426214331332,-0.375090745122094));
#8329=CARTESIAN_POINT('Ctrl Pts',(80.5546209258193,-3.39869986199205,-0.746677677909009));
#8330=CARTESIAN_POINT('Ctrl Pts',(80.5727447454929,-3.28132205985502,-1.09758759467381));
#8331=CARTESIAN_POINT('Ctrl Pts',(80.6285745144992,-2.91974399861838,-2.17855286291426));
#8332=CARTESIAN_POINT('Ctrl Pts',(80.6844042835056,-1.97158258973338,-3.06330861746674));
#8333=CARTESIAN_POINT('Ctrl Pts',(80.7402340525119,-0.868215259536808,-3.34932459633046));
#8334=CARTESIAN_POINT('Ctrl Pts',(80.7960638215183,0.235152070659761,-3.63534057519418));
#8335=CARTESIAN_POINT('Ctrl Pts',(80.8518935905247,1.4937253221679,-3.32261677836914));
#8336=CARTESIAN_POINT('Ctrl Pts',(80.907723359531,2.33490147085537,-2.5534306549958));
#8337=CARTESIAN_POINT('Ctrl Pts',(80.9635531285374,3.17607761954284,-1.78424453162245));
#8338=CARTESIAN_POINT('Ctrl Pts',(81.0193828975437,3.59985666540964,-0.558596081700797));
#8339=CARTESIAN_POINT('Ctrl Pts',(81.0752126665501,3.41343523929463,0.565891204752768));
#8340=CARTESIAN_POINT('Ctrl Pts',(81.1310424355564,3.22701381317962,1.69037849120633));
#8341=CARTESIAN_POINT('Ctrl Pts',(81.1868722045628,2.4303919150828,2.7137046141918));
#8342=CARTESIAN_POINT('Ctrl Pts',(81.2427019735692,1.3860022499685,3.17029505749191));
#8343=CARTESIAN_POINT('Ctrl Pts',(81.2985317425755,0.341612584854186,3.62688550079202));
#8344=CARTESIAN_POINT('Ctrl Pts',(81.3543615115819,-0.950544847277621,3.51674026440676));
#8345=CARTESIAN_POINT('Ctrl Pts',(81.4101912805883,-1.90258749576358,2.88997124716479));
#8346=CARTESIAN_POINT('Ctrl Pts',(81.4656963936607,-2.84909391687946,2.26684695717687));
#8347=CARTESIAN_POINT('Ctrl Pts',(81.521201506733,-3.45942965915134,1.13308985888859));
#8348=CARTESIAN_POINT('Ctrl Pts',(81.5767066198053,-3.46001944289485,-0.000122141770493717));
#8349=CARTESIAN_POINT('Ctrl Pts',(81.2792421631699,-3.44913158907647,0.00100292261883378));
#8350=CARTESIAN_POINT('Ctrl Pts',(81.2543892656095,-3.45047091392514,0.512534652402619));
#8351=CARTESIAN_POINT('Ctrl Pts',(81.2295363680491,-3.3438907635004,1.02353572618038));
#8352=CARTESIAN_POINT('Ctrl Pts',(81.2046834704887,-3.12655411418531,1.48203645516729));
#8353=CARTESIAN_POINT('Ctrl Pts',(81.1488537014823,-2.63832714192235,2.51201655009872));
#8354=CARTESIAN_POINT('Ctrl Pts',(81.093023932476,-1.59118381050591,3.27706138742638));
#8355=CARTESIAN_POINT('Ctrl Pts',(81.0371941634696,-0.461534561322807,3.42910462542053));
#8356=CARTESIAN_POINT('Ctrl Pts',(80.9813643944633,0.668114687860321,3.58114786341467));
#8357=CARTESIAN_POINT('Ctrl Pts',(80.9255346254569,1.88026985481012,3.12018950207527));
#8358=CARTESIAN_POINT('Ctrl Pts',(80.8697048564505,2.62344638073682,2.25594808689628));
#8359=CARTESIAN_POINT('Ctrl Pts',(80.8138750874442,3.36662290666352,1.39170667171732));
#8360=CARTESIAN_POINT('Ctrl Pts',(80.7580453184378,3.64082079156714,0.124182202698778));
#8361=CARTESIAN_POINT('Ctrl Pts',(80.7022155494315,3.32129041287442,-0.969949832064032));
#8362=CARTESIAN_POINT('Ctrl Pts',(80.6463857804251,3.0017600341817,-2.06408186682685));
#8363=CARTESIAN_POINT('Ctrl Pts',(80.5905560114187,2.08850139189263,-2.98482146733395));
#8364=CARTESIAN_POINT('Ctrl Pts',(80.5347262424124,0.997012479280798,-3.31326708847092));
#8365=CARTESIAN_POINT('Ctrl Pts',(80.478896473406,-0.0944764333310358,-3.64171270960789));
#8366=CARTESIAN_POINT('Ctrl Pts',(80.4230667043997,-1.36419561626563,-3.37786435137473));
#8367=CARTESIAN_POINT('Ctrl Pts',(80.3672369353933,-2.23447106995624,-2.64176299483581));
#8368=CARTESIAN_POINT('Ctrl Pts',(80.3184609002077,-2.99479279268316,-1.99866333123865));
#8369=CARTESIAN_POINT('Ctrl Pts',(80.2696848650221,-3.45022889886461,-0.995104519048995));
#8370=CARTESIAN_POINT('Ctrl Pts',(80.2209088298365,-3.45793510972046,0.00231429949518289));
#8371=CARTESIAN_POINT('Origin',(84.65,0.,0.));
#8372=CARTESIAN_POINT('',(79.1625754965032,-3.45582574002253,-0.002961649045852));
#8373=CARTESIAN_POINT('',(79.4600399531387,-3.45067402916032,0.00235956821323163));
#8374=CARTESIAN_POINT('',(84.65,-3.4544,-4.23041990297462E-16));
#8375=CARTESIAN_POINT('Ctrl Pts',(79.4600399531387,-3.45067402916032,0.00235956821323163));
#8376=CARTESIAN_POINT('Ctrl Pts',(79.4959629365519,-3.44599371542453,-0.736192453848879));
#8377=CARTESIAN_POINT('Ctrl Pts',(79.5318859199652,-3.21354307753759,-1.47743314832035));
#8378=CARTESIAN_POINT('Ctrl Pts',(79.5678089033784,-2.77566385451523,-2.06578390812058));
#8379=CARTESIAN_POINT('Ctrl Pts',(79.6236386723848,-2.09513307585447,-2.98017029514507));
#8380=CARTESIAN_POINT('Ctrl Pts',(79.6794684413911,-0.918412601109804,-3.52526820087666));
#8381=CARTESIAN_POINT('Ctrl Pts',(79.7352982103975,0.219134449978267,-3.4530787829694));
#8382=CARTESIAN_POINT('Ctrl Pts',(79.7911279794038,1.35668150106635,-3.38088936506215));
#8383=CARTESIAN_POINT('Ctrl Pts',(79.8469577484102,2.45505512849783,-2.69141262351603));
#8384=CARTESIAN_POINT('Ctrl Pts',(79.9027875174166,3.0145370520976,-1.69833428688242));
#8385=CARTESIAN_POINT('Ctrl Pts',(79.9586172864229,3.57401897569738,-0.705255950248812));
#8386=CARTESIAN_POINT('Ctrl Pts',(80.0144470554293,3.59460919546544,0.591423981472296));
#8387=CARTESIAN_POINT('Ctrl Pts',(80.0702768244356,3.06693994351031,1.60176539210869));
#8388=CARTESIAN_POINT('Ctrl Pts',(80.126106593442,2.53927069155519,2.61210680274506));
#8389=CARTESIAN_POINT('Ctrl Pts',(80.1819363624483,1.46334196787692,3.33610969229675));
#8390=CARTESIAN_POINT('Ctrl Pts',(80.2377661314547,0.328660473959983,3.4443802463351));
#8391=CARTESIAN_POINT('Ctrl Pts',(80.293595900461,-0.806021019956969,3.55265080037346));
#8392=CARTESIAN_POINT('Ctrl Pts',(80.3494256694675,-1.99945528411258,3.04518901889848));
#8393=CARTESIAN_POINT('Ctrl Pts',(80.4052554384738,-2.70867505939625,2.15287073719677));
#8394=CARTESIAN_POINT('Ctrl Pts',(80.4429613878066,-3.1876633373092,1.55022257086274));
#8395=CARTESIAN_POINT('Ctrl Pts',(80.4806673371393,-3.44578713492097,0.772030027260836));
#8396=CARTESIAN_POINT('Ctrl Pts',(80.5183732864721,-3.45151093143175,-0.00270500195080525));
#8397=CARTESIAN_POINT('Ctrl Pts',(80.2209088298365,-3.45793510972046,0.00231429949518289));
#8398=CARTESIAN_POINT('Ctrl Pts',(80.2138550960157,-3.45904954142728,0.14655576617193));
#8399=CARTESIAN_POINT('Ctrl Pts',(80.206801362195,-3.45080040796966,0.290668824557857));
#8400=CARTESIAN_POINT('Ctrl Pts',(80.1997476283742,-3.4327556926168,0.433544736072098));
#8401=CARTESIAN_POINT('Ctrl Pts',(80.1439178593678,-3.28993313714013,1.56439675559642));
#8402=CARTESIAN_POINT('Ctrl Pts',(80.0880880903615,-2.53345630174016,2.61774643980037));
#8403=CARTESIAN_POINT('Ctrl Pts',(80.0322583213552,-1.50749341271405,3.1143596924703));
#8404=CARTESIAN_POINT('Ctrl Pts',(79.9764285523488,-0.481530523687946,3.61097294514022));
#8405=CARTESIAN_POINT('Ctrl Pts',(79.9205987833424,0.813918418964297,3.55084976627612));
#8406=CARTESIAN_POINT('Ctrl Pts',(79.8647690143361,1.78947335231774,2.96134391865517));
#8407=CARTESIAN_POINT('Ctrl Pts',(79.8089392453297,2.76502828567118,2.37183807103423));
#8408=CARTESIAN_POINT('Ctrl Pts',(79.7531094763234,3.42068920972583,1.25294955465644));
#8409=CARTESIAN_POINT('Ctrl Pts',(79.697279707317,3.45815530848054,0.113730144726209));
#8410=CARTESIAN_POINT('Ctrl Pts',(79.6414499383106,3.49562140723526,-1.02548926520403));
#8411=CARTESIAN_POINT('Ctrl Pts',(79.5856201693043,2.91489268069002,-2.18503956868671));
#8412=CARTESIAN_POINT('Ctrl Pts',(79.5297904002979,1.98017864118596,-2.83736942130582));
#8413=CARTESIAN_POINT('Ctrl Pts',(79.4739606312915,1.0454646016819,-3.48969927392492));
#8414=CARTESIAN_POINT('Ctrl Pts',(79.4181308622852,-0.243234750780984,-3.63480867568044));
#8415=CARTESIAN_POINT('Ctrl Pts',(79.3623010932788,-1.29961016044813,-3.20667836130879));
#8416=CARTESIAN_POINT('Ctrl Pts',(79.3064713242725,-2.35598557011526,-2.77854804693713));
#8417=CARTESIAN_POINT('Ctrl Pts',(79.2506415552661,-3.18003703698667,-1.77717801643833));
#8418=CARTESIAN_POINT('Ctrl Pts',(79.1948117862598,-3.39685244416281,-0.658153596465372));
#8419=CARTESIAN_POINT('Ctrl Pts',(79.1840663563409,-3.43858241734022,-0.442777486259295));
#8420=CARTESIAN_POINT('Ctrl Pts',(79.1733209264221,-3.45781803868262,-0.223043006372249));
#8421=CARTESIAN_POINT('Ctrl Pts',(79.1625754965032,-3.45582574002253,-0.002961649045852));
#8422=CARTESIAN_POINT('Origin',(84.65,0.,0.));
#8423=CARTESIAN_POINT('',(78.1042421631699,-3.44886665199893,0.000209781305364476));
#8424=CARTESIAN_POINT('',(78.4017066198053,-3.45980363531856,0.000782824143658126));
#8425=CARTESIAN_POINT('',(84.65,-3.4544,-4.23041990297462E-16));
#8426=CARTESIAN_POINT('Ctrl Pts',(78.4017066198053,-3.45980363531856,0.000782824143658126));
#8427=CARTESIAN_POINT('Ctrl Pts',(78.4554287669582,-3.45641942945665,-1.09621141280894));
#8428=CARTESIAN_POINT('Ctrl Pts',(78.5091509141111,-2.88987735601417,-2.19621591060466));
#8429=CARTESIAN_POINT('Ctrl Pts',(78.5628730612639,-1.99338590411892,-2.82810636555822));
#8430=CARTESIAN_POINT('Ctrl Pts',(78.6187028302703,-1.06172339008944,-3.48478708304715));
#8431=CARTESIAN_POINT('Ctrl Pts',(78.6745325992766,0.226285422716833,-3.63590325801604));
#8432=CARTESIAN_POINT('Ctrl Pts',(78.730362368283,1.28464545005932,-3.21270276560162));
#8433=CARTESIAN_POINT('Ctrl Pts',(78.7861921372894,2.3430054774018,-2.7895022731872));
#8434=CARTESIAN_POINT('Ctrl Pts',(78.8420219062958,3.1717167192805,-1.79198511338946));
#8435=CARTESIAN_POINT('Ctrl Pts',(78.8978516753021,3.39374703706223,-0.673983707137805));
#8436=CARTESIAN_POINT('Ctrl Pts',(78.9536814443085,3.61577735484395,0.44401769911385));
#8437=CARTESIAN_POINT('Ctrl Pts',(79.0095112133148,3.23112674852871,1.68250335181942));
#8438=CARTESIAN_POINT('Ctrl Pts',(79.0653409823211,2.4147966340945,2.47800932264061));
#8439=CARTESIAN_POINT('Ctrl Pts',(79.1211707513275,1.59846651966029,3.2735152934618));
#8440=CARTESIAN_POINT('Ctrl Pts',(79.1770005203339,0.350456897107113,3.62604158239858));
#8441=CARTESIAN_POINT('Ctrl Pts',(79.2328302893402,-0.761435259650085,3.37520211756753));
#8442=CARTESIAN_POINT('Ctrl Pts',(79.2886600583466,-1.87332741640728,3.12436265273647));
#8443=CARTESIAN_POINT('Ctrl Pts',(79.3444898273529,-2.84910210736849,2.27015743413759));
#8444=CARTESIAN_POINT('Ctrl Pts',(79.4003195963593,-3.24481891156067,1.20121739067945));
#8445=CARTESIAN_POINT('Ctrl Pts',(79.4202263819524,-3.3859165681846,0.820073770783605));
#8446=CARTESIAN_POINT('Ctrl Pts',(79.4401331675456,-3.45326763339901,0.411629493916263));
#8447=CARTESIAN_POINT('Ctrl Pts',(79.4600399531387,-3.45067402916032,0.00235956821323163));
#8448=CARTESIAN_POINT('Ctrl Pts',(79.1625754965032,-3.45582574002253,-0.002961649045852));
#8449=CARTESIAN_POINT('Ctrl Pts',(79.1174911574157,-3.44746670096746,0.920428351678523));
#8450=CARTESIAN_POINT('Ctrl Pts',(79.0724068183282,-3.06541784343642,1.84992467687227));
#8451=CARTESIAN_POINT('Ctrl Pts',(79.0273224792407,-2.40321705390905,2.48924094437753));
#8452=CARTESIAN_POINT('Ctrl Pts',(78.9714927102343,-1.58318690899829,3.28093225580035));
#8453=CARTESIAN_POINT('Ctrl Pts',(78.915662941228,-0.333547271695907,3.62763606919886));
#8454=CARTESIAN_POINT('Ctrl Pts',(78.8598331722216,0.777163289075481,3.3716153242409));
#8455=CARTESIAN_POINT('Ctrl Pts',(78.8040034032152,1.88787384984687,3.11559457928293));
#8456=CARTESIAN_POINT('Ctrl Pts',(78.7481736342089,2.85965533408728,2.25684927596851));
#8457=CARTESIAN_POINT('Ctrl Pts',(78.6923438652025,3.25038407819797,1.18607589779917));
#8458=CARTESIAN_POINT('Ctrl Pts',(78.6365140961962,3.64111282230867,0.115302519629842));
#8459=CARTESIAN_POINT('Ctrl Pts',(78.5806843271898,3.45078882628966,-1.1674989333944));
#8460=CARTESIAN_POINT('Ctrl Pts',(78.5248545581834,2.76600227941643,-2.07870250373423));
#8461=CARTESIAN_POINT('Ctrl Pts',(78.4690247891771,2.0812157325432,-2.98990607407406));
#8462=CARTESIAN_POINT('Ctrl Pts',(78.4131950201707,0.901966634815757,-3.52951176172949));
#8463=CARTESIAN_POINT('Ctrl Pts',(78.3573652511644,-0.235231467171954,-3.45201951840901));
#8464=CARTESIAN_POINT('Ctrl Pts',(78.301535482158,-1.37242956915966,-3.37452727508854));
#8465=CARTESIAN_POINT('Ctrl Pts',(78.2457057131517,-2.46757667540763,-2.67993710079217));
#8466=CARTESIAN_POINT('Ctrl Pts',(78.1898759441453,-3.02242244917052,-1.68426105623825));
#8467=CARTESIAN_POINT('Ctrl Pts',(78.1613313504868,-3.30610349311992,-1.17519271128376));
#8468=CARTESIAN_POINT('Ctrl Pts',(78.1327867568284,-3.44854635896393,-0.587418619717722));
#8469=CARTESIAN_POINT('Ctrl Pts',(78.1042421631699,-3.44886665199893,0.000209781305364476));
#8470=CARTESIAN_POINT('Origin',(84.65,0.,0.));
#8471=CARTESIAN_POINT('',(77.0459088298365,-3.45658164681457,0.00280094662916092));
#8472=CARTESIAN_POINT('',(77.343373286472,-3.45282914603924,-0.00301189592616661));
#8473=CARTESIAN_POINT('',(84.65,-3.4544,-4.23041990297462E-16));
#8474=CARTESIAN_POINT('Ctrl Pts',(77.343373286472,-3.45282914603924,-0.00301189592616661));
#8475=CARTESIAN_POINT('Ctrl Pts',(77.3590648283581,-3.45555696923012,-0.325110759859066));
#8476=CARTESIAN_POINT('Ctrl Pts',(77.3747563702442,-3.41414927856796,-0.646521813152243));
#8477=CARTESIAN_POINT('Ctrl Pts',(77.3904479121303,-3.32577665812594,-0.954454511638704));
#8478=CARTESIAN_POINT('Ctrl Pts',(77.4462776811367,-3.01135102541417,-2.05006458939772));
#8479=CARTESIAN_POINT('Ctrl Pts',(77.5021074501431,-2.10239494861453,-2.97505177244844));
#8480=CARTESIAN_POINT('Ctrl Pts',(77.5579372191495,-1.01244917268523,-3.30858262931605));
#8481=CARTESIAN_POINT('Ctrl Pts',(77.6137669881558,0.0774966032440712,-3.64211348618366));
#8482=CARTESIAN_POINT('Ctrl Pts',(77.6695967571622,1.34843207830302,-3.38418801686816));
#8483=CARTESIAN_POINT('Ctrl Pts',(77.7254265261685,2.22213001584954,-2.65215220736641));
#8484=CARTESIAN_POINT('Ctrl Pts',(77.7812562951749,3.09582795339607,-1.92011639786466));
#8485=CARTESIAN_POINT('Ctrl Pts',(77.8370860641813,3.57228835343016,-0.713970248176632));
#8486=CARTESIAN_POINT('Ctrl Pts',(77.8929158331876,3.43473976591166,0.41753540250213));
#8487=CARTESIAN_POINT('Ctrl Pts',(77.948745602194,3.29719117839316,1.54904105318089));
#8488=CARTESIAN_POINT('Ctrl Pts',(78.0045753712003,2.54563360332207,2.60590620485039));
#8489=CARTESIAN_POINT('Ctrl Pts',(78.0604051402067,1.52199722376043,3.10729743581821));
#8490=CARTESIAN_POINT('Ctrl Pts',(78.116234909213,0.498360844198792,3.60868866678604));
#8491=CARTESIAN_POINT('Ctrl Pts',(78.1720646782194,-0.797354339853391,3.55460597705218));
#8492=CARTESIAN_POINT('Ctrl Pts',(78.2278944472258,-1.77564715267084,2.9696548962903));
#8493=CARTESIAN_POINT('Ctrl Pts',(78.2837242162321,-2.7539399654883,2.38470381552842));
#8494=CARTESIAN_POINT('Ctrl Pts',(78.3395539852385,-3.41481040707101,1.26888434373852));
#8495=CARTESIAN_POINT('Ctrl Pts',(78.3953837542448,-3.45758752023603,0.129851977839085));
#8496=CARTESIAN_POINT('Ctrl Pts',(78.3974913760983,-3.45920239309224,0.0868525252361583));
#8497=CARTESIAN_POINT('Ctrl Pts',(78.3995989979518,-3.45993640414128,0.0438199912992089));
#8498=CARTESIAN_POINT('Ctrl Pts',(78.4017066198053,-3.45980363531856,0.000782824143658126));
#8499=CARTESIAN_POINT('Ctrl Pts',(78.1042421631699,-3.44886665199893,0.000209781305364476));
#8500=CARTESIAN_POINT('Ctrl Pts',(78.076956987822,-3.4491728133592,0.561911382426732));
#8501=CARTESIAN_POINT('Ctrl Pts',(78.0496718124741,-3.3196209391107,1.12347986544209));
#8502=CARTESIAN_POINT('Ctrl Pts',(78.0223866371262,-3.0594386069859,1.61604710434839));
#8503=CARTESIAN_POINT('Ctrl Pts',(77.9665568681198,-2.52706454976058,2.62391730556962));
#8504=CARTESIAN_POINT('Ctrl Pts',(77.9107270991135,-1.44777199403211,3.34289579320058));
#8505=CARTESIAN_POINT('Ctrl Pts',(77.8548973301072,-0.312598052546025,3.44587499691791));
#8506=CARTESIAN_POINT('Ctrl Pts',(77.7990675611008,0.822575888940055,3.54885420063523));
#8507=CARTESIAN_POINT('Ctrl Pts',(77.7432377920944,2.01363121618376,3.03583412043895));
#8508=CARTESIAN_POINT('Ctrl Pts',(77.687408023088,2.7186829870306,2.14021875184474));
#8509=CARTESIAN_POINT('Ctrl Pts',(77.6315782540817,3.42373475787744,1.24460338325053));
#8510=CARTESIAN_POINT('Ctrl Pts',(77.5757484850753,3.64278297232741,-0.0336072737416136));
#8511=CARTESIAN_POINT('Ctrl Pts',(77.519918716069,3.27616903077557,-1.11287463115828));
#8512=CARTESIAN_POINT('Ctrl Pts',(77.4640889470626,2.90955508922373,-2.19214198857496));
#8513=CARTESIAN_POINT('Ctrl Pts',(77.4082591780563,1.95727899167008,-3.07246604641616));
#8514=CARTESIAN_POINT('Ctrl Pts',(77.3524294090499,0.852590156611448,-3.35333533965697));
#8515=CARTESIAN_POINT('Ctrl Pts',(77.2965996400435,-0.252098678447182,-3.63420463289779));
#8516=CARTESIAN_POINT('Ctrl Pts',(77.2407698710372,-1.50920025101079,-3.31561916153822));
#8517=CARTESIAN_POINT('Ctrl Pts',(77.1849401020308,-2.34678102618597,-2.5425182006909));
#8518=CARTESIAN_POINT('Ctrl Pts',(77.1385963446327,-3.04204881856385,-1.90077448561923));
#8519=CARTESIAN_POINT('Ctrl Pts',(77.0922525872346,-3.44824574888005,-0.945846811171742));
#8520=CARTESIAN_POINT('Ctrl Pts',(77.0459088298365,-3.45658164681457,0.00280094662916092));
#8521=CARTESIAN_POINT('Origin',(84.65,0.,0.));
#8522=CARTESIAN_POINT('',(75.9875754965032,-3.45725565822888,-0.00252520199929829));
#8523=CARTESIAN_POINT('',(76.2850399531387,-3.44974973462971,0.00177277111675968));
#8524=CARTESIAN_POINT('',(84.65,-3.4544,-4.23041990297462E-16));
#8525=CARTESIAN_POINT('',(75.342557724821,2.66903922910597,-2.19296806941949));
#8526=CARTESIAN_POINT('Ctrl Pts',(75.9875754965032,-3.45725565822888,-0.00252520199929829));
#8527=CARTESIAN_POINT('Ctrl Pts',(75.9400588796282,-3.44912275835016,0.969407753130569));
#8528=CARTESIAN_POINT('Ctrl Pts',(75.8925422627532,-3.01962093091058,1.94744243616048));
#8529=CARTESIAN_POINT('Ctrl Pts',(75.8450256458782,-2.29316705426671,2.59066122337652));
#8530=CARTESIAN_POINT('Ctrl Pts',(75.7891958768718,-1.4396182371553,3.34641276194424));
#8531=CARTESIAN_POINT('Ctrl Pts',(75.7333661078655,-0.176123125833669,3.63994645726298));
#8532=CARTESIAN_POINT('Ctrl Pts',(75.6775363388591,0.92247066266989,3.33539582878245));
#8533=CARTESIAN_POINT('Ctrl Pts',(75.6217065698528,2.02106445117345,3.03084520030191));
#8534=CARTESIAN_POINT('Ctrl Pts',(75.5658768008464,2.95475691685894,2.12821024802208));
#8535=CARTESIAN_POINT('Ctrl Pts',(75.5100470318401,3.29846760420812,1.04342284236128));
#8536=CARTESIAN_POINT('Ctrl Pts',(75.4542172628337,3.64217829155731,-0.0413645632995172));
#8537=CARTESIAN_POINT('Ctrl Pts',(75.3983874938273,3.3959072005702,-1.30830442234129));
#8538=CARTESIAN_POINT('Ctrl Pts',(75.342557724821,2.66903922910596,-2.1929680694195));
#8539=CARTESIAN_POINT('',(75.342557724821,-2.66725710276986,-2.19542711810056));
#8540=CARTESIAN_POINT('Origin',(75.342557724821,0.,0.));
#8541=CARTESIAN_POINT('Ctrl Pts',(75.342557724821,-2.66725710276986,-2.19542711810056));
#8542=CARTESIAN_POINT('Ctrl Pts',(75.3552305591811,-2.5042708137433,-2.39790962253998));
#8543=CARTESIAN_POINT('Ctrl Pts',(75.3679033935413,-2.31900993594976,-2.58145235087825));
#8544=CARTESIAN_POINT('Ctrl Pts',(75.3805762279015,-2.11423969877341,-2.73967296209481));
#8545=CARTESIAN_POINT('Ctrl Pts',(75.4364059969078,-1.21213092688924,-3.43670883625072));
#8546=CARTESIAN_POINT('Ctrl Pts',(75.4922357659142,0.0686184225984726,-3.64228925741259));
#8547=CARTESIAN_POINT('Ctrl Pts',(75.5480655349206,1.14443454333613,-3.26502848098788));
#8548=CARTESIAN_POINT('Ctrl Pts',(75.6038953039269,2.22025066407378,-2.88776770456317));
#8549=CARTESIAN_POINT('Ctrl Pts',(75.6597250729332,3.09113355606137,-1.92766573055188));
#8550=CARTESIAN_POINT('Ctrl Pts',(75.7155548419396,3.36131099418083,-0.820474311753891));
#8551=CARTESIAN_POINT('Ctrl Pts',(75.7713846109459,3.63148843230029,0.286717107044106));
#8552=CARTESIAN_POINT('Ctrl Pts',(75.8272143799524,3.3009604165516,1.54099797062881));
#8553=CARTESIAN_POINT('Ctrl Pts',(75.8830441489587,2.51987823294149,2.37118396395587));
#8554=CARTESIAN_POINT('Ctrl Pts',(75.9388739179651,1.73879604933139,3.20136995728294));
#8555=CARTESIAN_POINT('Ctrl Pts',(75.9947036869714,0.507159697859874,3.60746108035237));
#8556=CARTESIAN_POINT('Ctrl Pts',(76.0505334559777,-0.614568213469516,3.4049720476312));
#8557=CARTESIAN_POINT('Ctrl Pts',(76.1063632249841,-1.73629612479891,3.20248301491003));
#8558=CARTESIAN_POINT('Ctrl Pts',(76.1621929939905,-2.74811559598618,2.39141382639824));
#8559=CARTESIAN_POINT('Ctrl Pts',(76.2180227629968,-3.18974546299614,1.34063282447457));
#8560=CARTESIAN_POINT('Ctrl Pts',(76.2403618263775,-3.366454014106,0.920185743662626));
#8561=CARTESIAN_POINT('Ctrl Pts',(76.2627008897581,-3.45187375359347,0.461360189413245));
#8562=CARTESIAN_POINT('Ctrl Pts',(76.2850399531387,-3.44974973462971,0.00177277111675968));
#8563=CARTESIAN_POINT('Origin',(73.0447820522122,0.,0.));
#8564=CARTESIAN_POINT('',(93.5153333974298,-3.96228178397161,0.000254737798764393));
#8565=CARTESIAN_POINT('',(93.6822820522122,-3.96673102035433,0.00521690610871163));
#8566=CARTESIAN_POINT('',(73.0447820522122,-3.96875,-4.10839266763092E-13));
#8567=CARTESIAN_POINT('',(93.8044,-2.97061198327647,-2.63181325464293));
#8568=CARTESIAN_POINT('Ctrl Pts',(93.6822820522122,-3.96673102035433,0.00521690610871168));
#8569=CARTESIAN_POINT('Ctrl Pts',(93.7229880348082,-3.95801329736185,-0.951787959283503));
#8570=CARTESIAN_POINT('Ctrl Pts',(93.7636940174041,-3.60663188570075,-1.91391720316181));
#8571=CARTESIAN_POINT('Ctrl Pts',(93.8044,-2.97061198327643,-2.63181325464298));
#8572=CARTESIAN_POINT('',(93.8044000000001,0.57142891900023,-3.92761210585551));
#8573=CARTESIAN_POINT('Origin',(93.8044,0.,0.));
#8574=CARTESIAN_POINT('Ctrl Pts',(93.5153333974298,-3.96228178397161,0.00025473779876474));
#8575=CARTESIAN_POINT('Ctrl Pts',(93.5431863282533,-3.96226415926583,-0.658364510072053));
#8576=CARTESIAN_POINT('Ctrl Pts',(93.6268690280832,-3.49522148123942,-2.63729827531904));
#8577=CARTESIAN_POINT('Ctrl Pts',(93.7232245622734,-1.34167057967468,-4.04359863780956));
#8578=CARTESIAN_POINT('Ctrl Pts',(93.7917271656399,0.27639455735742,-3.97383332500728));
#8579=CARTESIAN_POINT('Ctrl Pts',(93.8044,0.57142891900023,-3.92761210585551));
#8580=CARTESIAN_POINT('Origin',(73.0447820522122,0.,0.));
#8581=CARTESIAN_POINT('',(92.4570000640964,-3.97078332034416,0.00332551191120287));
#8582=CARTESIAN_POINT('',(92.6239487188789,-3.97480878038019,-0.00116026438185279));
#8583=CARTESIAN_POINT('',(73.0447820522122,-3.96875,-4.10839266763092E-13));
#8584=CARTESIAN_POINT('Ctrl Pts',(92.6239487188789,-3.97480878038019,-0.00116026438185197));
#8585=CARTESIAN_POINT('Ctrl Pts',(92.626624096208,-3.97504728960825,-0.0639306450881609));
#8586=CARTESIAN_POINT('Ctrl Pts',(92.6851292425436,-3.94532727312447,-1.43635923310198));
#8587=CARTESIAN_POINT('Ctrl Pts',(92.7994641578856,-2.36394076440595,-4.0456605360623));
#8588=CARTESIAN_POINT('Ctrl Pts',(92.9669534649047,2.10367480928929,-4.18746581500559));
#8589=CARTESIAN_POINT('Ctrl Pts',(93.1344427719237,4.65703774727922,-0.51765171101067));
#8590=CARTESIAN_POINT('Ctrl Pts',(93.3019320789428,2.97298396264366,3.62053493698499));
#8591=CARTESIAN_POINT('Ctrl Pts',(93.4694213859619,-1.41651251429978,4.46956712243346));
#8592=CARTESIAN_POINT('Ctrl Pts',(93.596204710385,-3.76325080247511,2.025591834054));
#8593=CARTESIAN_POINT('Ctrl Pts',(93.6671582658018,-3.96996997866256,0.360779805095954));
#8594=CARTESIAN_POINT('Ctrl Pts',(93.6822820522122,-3.96673102035433,0.00521690610871168));
#8595=CARTESIAN_POINT('Ctrl Pts',(92.4570000640964,-3.97078332034416,0.0033255119112029));
#8596=CARTESIAN_POINT('Ctrl Pts',(92.5026521586596,-3.9611636135282,-1.07063415837227));
#8597=CARTESIAN_POINT('Ctrl Pts',(92.6041340222292,-2.95791654582123,-3.47380932989873));
#8598=CARTESIAN_POINT('Ctrl Pts',(92.761445654805,1.09859778933808,-4.55527773120639));
#8599=CARTESIAN_POINT('Ctrl Pts',(92.9289349618241,4.4179760167816,-1.56159205661129));
#8600=CARTESIAN_POINT('Ctrl Pts',(93.0964242688432,3.71721744660719,2.85269706473892));
#8601=CARTESIAN_POINT('Ctrl Pts',(93.2639135758623,-0.365701395163535,4.67189257704037));
#8602=CARTESIAN_POINT('Ctrl Pts',(93.4035499520579,-3.49259078967768,2.64337465166492));
#8603=CARTESIAN_POINT('Ctrl Pts',(93.487356559247,-3.96229948708317,0.661803938436363));
#8604=CARTESIAN_POINT('Ctrl Pts',(93.5153333974298,-3.96228178397161,0.00025473779876474));
#8605=CARTESIAN_POINT('Origin',(73.0447820522122,0.,0.));
#8606=CARTESIAN_POINT('',(91.3986667307631,-3.97246823586828,-0.00280997941530858));
#8607=CARTESIAN_POINT('',(91.5656153855456,-3.96419497404471,-0.00256333403586442));
#8608=CARTESIAN_POINT('',(73.0447820522122,-3.96875,-4.10839266763092E-13));
#8609=CARTESIAN_POINT('Ctrl Pts',(91.5656153855456,-3.96419497404471,-0.00256333403586429));
#8610=CARTESIAN_POINT('Ctrl Pts',(91.5860899266144,-3.96707960586625,-0.486267227833301));
#8611=CARTESIAN_POINT('Ctrl Pts',(91.6623942366896,-3.66153217022063,-2.28541151142624));
#8612=CARTESIAN_POINT('Ctrl Pts',(91.7945283157709,-0.984921998283766,-4.58115525704141));
#8613=CARTESIAN_POINT('Ctrl Pts',(91.9620176227903,3.30407582270753,-3.32268146160252));
#8614=CARTESIAN_POINT('Ctrl Pts',(92.1295069298092,4.58661448010922,0.959202947931876));
#8615=CARTESIAN_POINT('Ctrl Pts',(92.2969962368283,1.69568469472483,4.36824040377796));
#8616=CARTESIAN_POINT('Ctrl Pts',(92.4618101665183,-2.66736966883454,3.81163512773909));
#8617=CARTESIAN_POINT('Ctrl Pts',(92.5707943272017,-3.97007007949167,1.24596153985253));
#8618=CARTESIAN_POINT('Ctrl Pts',(92.6239487188789,-3.97480878038019,-0.00116026438185197));
#8619=CARTESIAN_POINT('Ctrl Pts',(91.3986667307631,-3.97246823586828,-0.00280997941530784));
#8620=CARTESIAN_POINT('Ctrl Pts',(91.4062882200596,-3.97390842000699,-0.181907740360926));
#8621=CARTESIAN_POINT('Ctrl Pts',(91.4697394783624,-3.88173674403366,-1.67146133766004));
#8622=CARTESIAN_POINT('Ctrl Pts',(91.5890205056715,-1.99881293045711,-4.2381396621777));
#8623=CARTESIAN_POINT('Ctrl Pts',(91.7565098126906,2.46387542085175,-3.98577567712814));
#8624=CARTESIAN_POINT('Ctrl Pts',(91.9239991197097,4.68462530132107,-0.10665579043167));
#8625=CARTESIAN_POINT('Ctrl Pts',(92.0914884267288,2.64272008949707,3.86950719504337));
#8626=CARTESIAN_POINT('Ctrl Pts',(92.2589777337479,-1.80385580473937,4.3247235657652));
#8627=CARTESIAN_POINT('Ctrl Pts',(92.3808149462037,-3.84445876308829,1.79327554700216));
#8628=CARTESIAN_POINT('Ctrl Pts',(92.4468223896532,-3.97292793704025,0.242753998025987));
#8629=CARTESIAN_POINT('Ctrl Pts',(92.4570000640964,-3.97078332034416,0.0033255119112029));
#8630=CARTESIAN_POINT('Origin',(73.0447820522122,0.,0.));
#8631=CARTESIAN_POINT('',(90.3403333974298,-3.96259069745009,-0.00094416610920911));
#8632=CARTESIAN_POINT('',(90.5072820522123,-3.96576562046892,0.0032106135516634));
#8633=CARTESIAN_POINT('',(73.0447820522122,-3.96875,-4.10839266763092E-13));
#8634=CARTESIAN_POINT('Ctrl Pts',(90.5072820522123,-3.96576562046892,0.00321061355166345));
#8635=CARTESIAN_POINT('Ctrl Pts',(90.5455557570207,-3.95882871231444,-0.900089954804321));
#8636=CARTESIAN_POINT('Ctrl Pts',(90.6396592308354,-3.20563741620691,-3.13149768310236));
#8637=CARTESIAN_POINT('Ctrl Pts',(90.7895924736566,0.492243639519289,-4.6599120176056));
#8638=CARTESIAN_POINT('Ctrl Pts',(90.9570817806758,4.17521467245732,-2.12712653204012));
#8639=CARTESIAN_POINT('Ctrl Pts',(91.1245710876947,4.05905751400097,2.34118289566344));
#8640=CARTESIAN_POINT('Ctrl Pts',(91.2920603947138,0.249466413298239,4.67919297252862));
#8641=CARTESIAN_POINT('Ctrl Pts',(91.4390751606641,-3.29367227435324,2.99416580689908));
#8642=CARTESIAN_POINT('Ctrl Pts',(91.5302601576081,-3.95921382134275,0.832691598517345));
#8643=CARTESIAN_POINT('Ctrl Pts',(91.5656153855456,-3.96419497404471,-0.00256333403586429));
#8644=CARTESIAN_POINT('Ctrl Pts',(90.3403333974298,-3.96259069745009,-0.000944166109208833));
#8645=CARTESIAN_POINT('Ctrl Pts',(90.3657540504659,-3.96387837288311,-0.602107582562329));
#8646=CARTESIAN_POINT('Ctrl Pts',(90.4470044725083,-3.55362928902476,-2.52190045542289));
#8647=CARTESIAN_POINT('Ctrl Pts',(90.584084663557,-0.578055276042246,-4.65004698078105));
#8648=CARTESIAN_POINT('Ctrl Pts',(90.7515739705762,3.58359009673503,-3.01910035578126));
#8649=CARTESIAN_POINT('Ctrl Pts',(90.9190632775952,4.48444073454358,1.35899828774903));
#8650=CARTESIAN_POINT('Ctrl Pts',(91.0865525846143,1.304790942286,4.5005116341675));
#8651=CARTESIAN_POINT('Ctrl Pts',(91.2464204023369,-2.8634060745579,3.59029486786392));
#8652=CARTESIAN_POINT('Ctrl Pts',(91.3504584510532,-3.96335862525385,1.13003881420564));
#8653=CARTESIAN_POINT('Ctrl Pts',(91.3986667307631,-3.97246823586828,-0.00280997941530784));
#8654=CARTESIAN_POINT('Origin',(73.0447820522122,0.,0.));
#8655=CARTESIAN_POINT('',(89.2820000640964,-3.9690716332801,0.00355215784508645));
#8656=CARTESIAN_POINT('',(89.4489487188789,-3.97520890573159,-0.000105091489476044));
#8657=CARTESIAN_POINT('',(73.0447820522122,-3.96875,-4.10839266763092E-13));
#8658=CARTESIAN_POINT('Ctrl Pts',(89.4489487188789,-3.97520890573159,-0.000105091489475756));
#8659=CARTESIAN_POINT('Ctrl Pts',(89.4491918184206,-3.97521113687027,-0.00580729351476086));
#8660=CARTESIAN_POINT('Ctrl Pts',(89.5052646869687,-3.97262415068171,-1.32106406366707));
#8661=CARTESIAN_POINT('Ctrl Pts',(89.617167324523,-2.53692607573313,-3.93968151281212));
#8662=CARTESIAN_POINT('Ctrl Pts',(89.7846566315422,1.9203526326146,-4.27426368987786));
#8663=CARTESIAN_POINT('Ctrl Pts',(89.9521459385612,4.63025632975995,-0.719590617471205));
#8664=CARTESIAN_POINT('Ctrl Pts',(90.1196352455803,3.12697851528032,3.48985525802016));
#8665=CARTESIAN_POINT('Ctrl Pts',(90.2871245525994,-1.22161219883188,4.5237979510226));
#8666=CARTESIAN_POINT('Ctrl Pts',(90.4163401548101,-3.71892401632552,2.14579381908193));
#8667=CARTESIAN_POINT('Ctrl Pts',(90.4897259880143,-3.96894756497898,0.417552597100143));
#8668=CARTESIAN_POINT('Ctrl Pts',(90.5072820522123,-3.96576562046892,0.00321061355166345));
#8669=CARTESIAN_POINT('Ctrl Pts',(89.2820000640964,-3.9690716332801,0.00355215784508672));
#8670=CARTESIAN_POINT('Ctrl Pts',(89.3252198808721,-3.95978931658861,-1.0143213554308));
#8671=CARTESIAN_POINT('Ctrl Pts',(89.4242694666542,-3.04365128022373,-3.36189206530121));
#8672=CARTESIAN_POINT('Ctrl Pts',(89.5791488214426,0.900310895961415,-4.59853511258327));
#8673=CARTESIAN_POINT('Ctrl Pts',(89.7466381284616,4.34616767952069,-1.75154543008276));
#8674=CARTESIAN_POINT('Ctrl Pts',(89.9141274354808,3.83734204230666,2.68921753416258));
#8675=CARTESIAN_POINT('Ctrl Pts',(90.0816167424998,-0.163173340857844,4.68299683371814));
#8676=CARTESIAN_POINT('Ctrl Pts',(90.2236853964828,-3.43057084216195,2.75973770851382));
#8677=CARTESIAN_POINT('Ctrl Pts',(90.3099242814595,-3.9610503329473,0.718189524991144));
#8678=CARTESIAN_POINT('Ctrl Pts',(90.3403333974298,-3.96259069745009,-0.000944166109208833));
#8679=CARTESIAN_POINT('Origin',(73.0447820522122,0.,0.));
#8680=CARTESIAN_POINT('',(88.223666730763,-3.97382271423798,-0.00207988543367732));
#8681=CARTESIAN_POINT('',(88.3906153855456,-3.96547802822572,-0.00312327481737352));
#8682=CARTESIAN_POINT('',(73.0447820522122,-3.96875,-4.10839266763092E-13));
#8683=CARTESIAN_POINT('Ctrl Pts',(88.3906153855456,-3.96547802822572,-0.00312327481737304));
#8684=CARTESIAN_POINT('Ctrl Pts',(88.4086576488269,-3.96864298053677,-0.429018094393009));
#8685=CARTESIAN_POINT('Ctrl Pts',(88.4825296811146,-3.70967706911612,-2.16905097144579));
#8686=CARTESIAN_POINT('Ctrl Pts',(88.6122314824085,-1.18239306112185,-4.53420676431444));
#8687=CARTESIAN_POINT('Ctrl Pts',(88.7797207894278,3.15708129655885,-3.46264667837653));
#8688=CARTESIAN_POINT('Ctrl Pts',(88.9472100964467,4.6238515098096,0.75965883636597));
#8689=CARTESIAN_POINT('Ctrl Pts',(89.1146994034659,1.88326811136568,4.29073251947842));
#8690=CARTESIAN_POINT('Ctrl Pts',(89.2819456109432,-2.56448120676564,3.91810719258513));
#8691=CARTESIAN_POINT('Ctrl Pts',(89.3933620494143,-3.97469873788979,1.30374935835586));
#8692=CARTESIAN_POINT('Ctrl Pts',(89.4489487188789,-3.97520890573159,-0.000105091489475756));
#8693=CARTESIAN_POINT('Ctrl Pts',(88.223666730763,-3.97382271423798,-0.00207988543367638));
#8694=CARTESIAN_POINT('Ctrl Pts',(88.228855942272,-3.97460074042894,-0.123912364854287));
#8695=CARTESIAN_POINT('Ctrl Pts',(88.2898749227873,-3.91438819662648,-1.55573883041568));
#8696=CARTESIAN_POINT('Ctrl Pts',(88.4067236723092,-2.18047806078814,-4.1476017550482));
#8697=CARTESIAN_POINT('Ctrl Pts',(88.574212979328,2.28895303198969,-4.08873805829862));
#8698=CARTESIAN_POINT('Ctrl Pts',(88.7417022863472,4.67561075159403,-0.309433339534459));
#8699=CARTESIAN_POINT('Ctrl Pts',(88.9091915933663,2.80781788150847,3.75143221135632));
#8700=CARTESIAN_POINT('Ctrl Pts',(89.0766809003853,-1.614875957977,4.39877943664814));
#8701=CARTESIAN_POINT('Ctrl Pts',(89.2009503906287,-3.80607569236581,1.90936693291494));
#8702=CARTESIAN_POINT('Ctrl Pts',(89.2693901118658,-3.97177987174111,0.300530195625075));
#8703=CARTESIAN_POINT('Ctrl Pts',(89.2820000640964,-3.9690716332801,0.00355215784508672));
#8704=CARTESIAN_POINT('Origin',(73.0447820522122,0.,0.));
#8705=CARTESIAN_POINT('',(87.1653333974297,-3.96319350967473,-0.00180240263408987));
#8706=CARTESIAN_POINT('',(87.3322820522123,-3.96442879726087,0.0026902431041884));
#8707=CARTESIAN_POINT('',(73.0447820522122,-3.96875,-4.10839266763092E-13));
#8708=CARTESIAN_POINT('Ctrl Pts',(87.3322820522123,-3.96442879726087,0.00269024310418864));
#8709=CARTESIAN_POINT('Ctrl Pts',(87.3681234792332,-3.95910818549169,-0.843925282767195));
#8710=CARTESIAN_POINT('Ctrl Pts',(87.4597946752604,-3.27938659012527,-3.01710310342379));
#8711=CARTESIAN_POINT('Ctrl Pts',(87.6072956402942,0.289976004112983,-4.67685773244287));
#8712=CARTESIAN_POINT('Ctrl Pts',(87.7747849473131,4.07917855433484,-2.3059459348224));
#8713=CARTESIAN_POINT('Ctrl Pts',(87.9422742543323,4.15663850493095,2.16320148663827));
#8714=CARTESIAN_POINT('Ctrl Pts',(88.1097635613514,0.451873185294068,4.66399988817462));
#8715=CARTESIAN_POINT('Ctrl Pts',(88.2592106050891,-3.22068607939857,3.10868133478913));
#8716=CARTESIAN_POINT('Ctrl Pts',(88.3528278798206,-3.95884938902959,0.888865866569467));
#8717=CARTESIAN_POINT('Ctrl Pts',(88.3906153855456,-3.96547802822572,-0.00312327481737304));
#8718=CARTESIAN_POINT('Ctrl Pts',(87.1653333974297,-3.96319350967473,-0.00180240263408953));
#8719=CARTESIAN_POINT('Ctrl Pts',(87.1883217726783,-3.96543626138576,-0.545238984627107));
#8720=CARTESIAN_POINT('Ctrl Pts',(87.2671399169332,-3.6083985865186,-2.40564992743396));
#8721=CARTESIAN_POINT('Ctrl Pts',(87.4017878301947,-0.778891559482246,-4.62065069342133));
#8722=CARTESIAN_POINT('Ctrl Pts',(87.5692771372135,3.44948051298471,-3.17146166342683));
#8723=CARTESIAN_POINT('Ctrl Pts',(87.7367664442328,4.53908736689592,1.16351655241039));
#8724=CARTESIAN_POINT('Ctrl Pts',(87.9042557512518,1.49846953985345,4.43978309494734));
#8725=CARTESIAN_POINT('Ctrl Pts',(88.066555846762,-2.76919203824914,3.69984238148232));
#8726=CARTESIAN_POINT('Ctrl Pts',(88.1730261732656,-3.96623010021758,1.18686079823135));
#8727=CARTESIAN_POINT('Ctrl Pts',(88.223666730763,-3.97382271423798,-0.00207988543367638));
#8728=CARTESIAN_POINT('Origin',(73.0447820522122,0.,0.));
#8729=CARTESIAN_POINT('',(86.1070000640964,-3.96737955141156,0.00351402329782577));
#8730=CARTESIAN_POINT('',(86.2739487188789,-3.97493882611752,0.00093324338624715));
#8731=CARTESIAN_POINT('',(73.0447820522122,-3.96875,-4.10839266763092E-13));
#8732=CARTESIAN_POINT('Ctrl Pts',(86.2739487188789,-3.97493882611752,0.000933243386247009));
#8733=CARTESIAN_POINT('Ctrl Pts',(86.3275893096394,-3.97092371063276,-1.25750325867978));
#8734=CARTESIAN_POINT('Ctrl Pts',(86.4370596694064,-2.6471458759135,-3.83301135212251));
#8735=CARTESIAN_POINT('Ctrl Pts',(86.6023597981797,1.7334463653411,-4.35341797108391));
#8736=CARTESIAN_POINT('Ctrl Pts',(86.7698491051987,4.59474916176048,-0.919437041331279));
#8737=CARTESIAN_POINT('Ctrl Pts',(86.9373384122179,3.27517927238433,3.35116174873949));
#8738=CARTESIAN_POINT('Ctrl Pts',(87.1048277192368,-1.02455494782308,4.5724579266913));
#8739=CARTESIAN_POINT('Ctrl Pts',(87.2364755992351,-3.67140987877257,2.26215094425435));
#8740=CARTESIAN_POINT('Ctrl Pts',(87.3122937102269,-3.96739603981938,0.47483775696838));
#8741=CARTESIAN_POINT('Ctrl Pts',(87.3322820522123,-3.96442879726087,0.00269024310418864));
#8742=CARTESIAN_POINT('Ctrl Pts',(86.1070000640964,-3.96737955141156,0.0035140232978258));
#8743=CARTESIAN_POINT('Ctrl Pts',(86.1477876030846,-3.9590346583871,-0.9581231290712));
#8744=CARTESIAN_POINT('Ctrl Pts',(86.2444049110792,-3.1253503766273,-3.24901199396521));
#8745=CARTESIAN_POINT('Ctrl Pts',(86.3968519880801,0.700318456568796,-4.63321043677455));
#8746=CARTESIAN_POINT('Ctrl Pts',(86.5643412950992,4.26623638905772,-1.93812073017321));
#8747=CARTESIAN_POINT('Ctrl Pts',(86.7318306021183,3.9502033026309,2.52051160678369));
#8748=CARTESIAN_POINT('Ctrl Pts',(86.8993199091373,0.0397852977070385,4.68566985842301));
#8749=CARTESIAN_POINT('Ctrl Pts',(87.0438208409079,-3.36514974078574,2.87524198487157));
#8750=CARTESIAN_POINT('Ctrl Pts',(87.132492003672,-3.95998949498269,0.774555847073451));
#8751=CARTESIAN_POINT('Ctrl Pts',(87.1653333974297,-3.96319350967473,-0.00180240263408953));
#8752=CARTESIAN_POINT('Origin',(73.0447820522122,0.,0.));
#8753=CARTESIAN_POINT('',(85.0486667307631,-3.97478647022473,-0.00116584238653683));
#8754=CARTESIAN_POINT('',(85.2156153855456,-3.96699920481957,-0.00346812739152993));
#8755=CARTESIAN_POINT('',(73.0447820522122,-3.96875,-4.10839266763092E-13));
#8756=CARTESIAN_POINT('Ctrl Pts',(85.2156153855455,-3.96699920481957,-0.00346812739152977));
#8757=CARTESIAN_POINT('Ctrl Pts',(85.2312253710394,-3.9701271390701,-0.371590363698427));
#8758=CARTESIAN_POINT('Ctrl Pts',(85.3026651255396,-3.75470286066849,-2.0527260743823));
#8759=CARTESIAN_POINT('Ctrl Pts',(85.4299346490461,-1.37764569709891,-4.47874722056687));
#8760=CARTESIAN_POINT('Ctrl Pts',(85.5974239560652,3.0041632824441,-3.59612114713693));
#8761=CARTESIAN_POINT('Ctrl Pts',(85.7649132630843,4.65241189360609,0.558701982011273));
#8762=CARTESIAN_POINT('Ctrl Pts',(85.9324025701033,2.06731911348409,4.20514875069765));
#8763=CARTESIAN_POINT('Ctrl Pts',(86.0998918771224,-2.39887701093383,4.02522961070344));
#8764=CARTESIAN_POINT('Ctrl Pts',(86.213740593381,-3.95098917456334,1.4132901908714));
#8765=CARTESIAN_POINT('Ctrl Pts',(86.2717595406331,-3.97510269089508,0.0522925176778244));
#8766=CARTESIAN_POINT('Ctrl Pts',(86.2739487188789,-3.97493882611752,0.000933243386247009));
#8767=CARTESIAN_POINT('Ctrl Pts',(85.0486667307631,-3.97478647022473,-0.00116584238653631));
#8768=CARTESIAN_POINT('Ctrl Pts',(85.0514236644845,-3.97503858705613,-0.0658515906554392));
#8769=CARTESIAN_POINT('Ctrl Pts',(85.1100103672124,-3.94436777223071,-1.44022332085691));
#8770=CARTESIAN_POINT('Ctrl Pts',(85.2244268389466,-2.35805169304712,-4.04928106025811));
#8771=CARTESIAN_POINT('Ctrl Pts',(85.3919161459656,2.10973547078508,-4.18402929427589));
#8772=CARTESIAN_POINT('Ctrl Pts',(85.5594054529847,4.65782362744017,-0.511628720565475));
#8773=CARTESIAN_POINT('Ctrl Pts',(85.7268947600037,2.96764612613796,3.62631512172698));
#8774=CARTESIAN_POINT('Ctrl Pts',(85.894384067023,-1.42286390542218,4.46458768518373));
#8775=CARTESIAN_POINT('Ctrl Pts',(86.0210858350537,-3.76477370815308,2.02558326012544));
#8776=CARTESIAN_POINT('Ctrl Pts',(86.0919578340782,-3.97045710410203,0.358160751165195));
#8777=CARTESIAN_POINT('Ctrl Pts',(86.1070000640964,-3.96737955141156,0.0035140232978258));
#8778=CARTESIAN_POINT('Origin',(73.0447820522122,0.,0.));
#8779=CARTESIAN_POINT('',(83.9903333974298,-3.9641570283979,-0.00254082259245281));
#8780=CARTESIAN_POINT('',(84.1572820522123,-3.96338763911034,0.00198750657534593));
#8781=CARTESIAN_POINT('',(73.0447820522122,-3.96875,-4.10839266763092E-13));
#8782=CARTESIAN_POINT('Ctrl Pts',(84.1572820522123,-3.96338763911034,0.00198750657534594));
#8783=CARTESIAN_POINT('Ctrl Pts',(84.1906912014457,-3.95978296584885,-0.787695341446297));
#8784=CARTESIAN_POINT('Ctrl Pts',(84.2799301196855,-3.34935300432391,-2.90214532004246));
#8785=CARTESIAN_POINT('Ctrl Pts',(84.4249988069316,0.0871642670565068,-4.68502793193585));
#8786=CARTESIAN_POINT('Ctrl Pts',(84.5924881139508,3.97548844210186,-2.48043866668484));
#8787=CARTESIAN_POINT('Ctrl Pts',(84.7599774209698,4.24642014257932,1.9811613526332));
#8788=CARTESIAN_POINT('Ctrl Pts',(84.9274667279889,0.653432103046516,4.64005504484363));
#8789=CARTESIAN_POINT('Ctrl Pts',(85.0793460495141,-3.14384921632806,3.22254157615712));
#8790=CARTESIAN_POINT('Ctrl Pts',(85.175395602033,-3.95893995079608,0.945014281914011));
#8791=CARTESIAN_POINT('Ctrl Pts',(85.2156153855455,-3.96699920481957,-0.00346812739152977));
#8792=CARTESIAN_POINT('Ctrl Pts',(83.9903333974298,-3.9641570283979,-0.00254082259245246));
#8793=CARTESIAN_POINT('Ctrl Pts',(84.0108894948909,-3.96702649059957,-0.488183074464591));
#8794=CARTESIAN_POINT('Ctrl Pts',(84.0872753613584,-3.65986279650672,-2.28931254822536));
#8795=CARTESIAN_POINT('Ctrl Pts',(84.219490996832,-0.97826636104911,-4.58258440390215));
#8796=CARTESIAN_POINT('Ctrl Pts',(84.3869803038513,3.30889846384542,-3.31787218681023));
#8797=CARTESIAN_POINT('Ctrl Pts',(84.5544696108702,4.58521705524031,0.965851669968393));
#8798=CARTESIAN_POINT('Ctrl Pts',(84.7219589178894,1.68933645364314,4.37072388037037));
#8799=CARTESIAN_POINT('Ctrl Pts',(84.886691291187,-2.67074242799831,3.80798725931741));
#8800=CARTESIAN_POINT('Ctrl Pts',(84.9955938954782,-3.96993305102157,1.24407847974412));
#8801=CARTESIAN_POINT('Ctrl Pts',(85.0486667307631,-3.97478647022473,-0.00116584238653631));
#8802=CARTESIAN_POINT('Origin',(73.0447820522122,0.,0.));
#8803=CARTESIAN_POINT('',(82.9320000640964,-3.96581480482491,0.00322439829302731));
#8804=CARTESIAN_POINT('',(83.0989487188788,-3.97408812184296,0.0018807273087504));
#8805=CARTESIAN_POINT('',(73.0447820522122,-3.96875,-4.10839266763092E-13));
#8806=CARTESIAN_POINT('Ctrl Pts',(83.0989487188788,-3.97408812184296,0.00188072730875047));
#8807=CARTESIAN_POINT('Ctrl Pts',(83.1501570318519,-3.9670176952052,-1.20017749285163));
#8808=CARTESIAN_POINT('Ctrl Pts',(83.2571951138316,-2.74659247719471,-3.72521760004062));
#8809=CARTESIAN_POINT('Ctrl Pts',(83.4200629648169,1.54328753190602,-4.42440368030926));
#8810=CARTESIAN_POINT('Ctrl Pts',(83.5875522718364,4.5506205990891,-1.11755827392429));
#8811=CARTESIAN_POINT('Ctrl Pts',(83.7550415788553,3.41723462017294,3.20618026367237));
#8812=CARTESIAN_POINT('Ctrl Pts',(83.9225308858744,-0.825575264478656,4.61253832668647));
#8813=CARTESIAN_POINT('Ctrl Pts',(84.05661104366,-3.62070390902415,2.37849907820253));
#8814=CARTESIAN_POINT('Ctrl Pts',(84.1348614324393,-3.96580670725351,0.531937513771429));
#8815=CARTESIAN_POINT('Ctrl Pts',(84.1572820522123,-3.96338763911034,0.00198750657534594));
#8816=CARTESIAN_POINT('Ctrl Pts',(82.9320000640964,-3.96581480482491,0.00322439829302756));
#8817=CARTESIAN_POINT('Ctrl Pts',(82.9703553252971,-3.95882711771097,-0.901972645909376));
#8818=CARTESIAN_POINT('Ctrl Pts',(83.0645403555041,-3.2030980355045,-3.13532234621704));
#8819=CARTESIAN_POINT('Ctrl Pts',(83.2145551547178,0.499011969014512,-4.65919219895763));
#8820=CARTESIAN_POINT('Ctrl Pts',(83.3820444617366,4.17830011134652,-2.12105942197974));
#8821=CARTESIAN_POINT('Ctrl Pts',(83.5495337687558,4.05565256718464,2.34707629751062));
#8822=CARTESIAN_POINT('Ctrl Pts',(83.7170230757749,0.242669284494185,4.67955088768255));
#8823=CARTESIAN_POINT('Ctrl Pts',(83.8639562853328,-3.29605384042193,2.99031534253484));
#8824=CARTESIAN_POINT('Ctrl Pts',(83.9550597258845,-3.959233113856,0.830807302627488));
#8825=CARTESIAN_POINT('Ctrl Pts',(83.9903333974298,-3.9641570283979,-0.00254082259245246));
#8826=CARTESIAN_POINT('Origin',(73.0447820522122,0.,0.));
#8827=CARTESIAN_POINT('',(81.873666730763,-3.97520616141411,-0.000140328321075467));
#8828=CARTESIAN_POINT('',(82.0406153855455,-3.96867065624537,-0.00356668729390831));
#8829=CARTESIAN_POINT('',(73.0447820522122,-3.96875,-4.10839266763092E-13));
#8830=CARTESIAN_POINT('Ctrl Pts',(82.0406153855455,-3.96867065624537,-0.00356668729390795));
#8831=CARTESIAN_POINT('Ctrl Pts',(82.0537930932519,-3.97148539159384,-0.313996266888609));
#8832=CARTESIAN_POINT('Ctrl Pts',(82.1228005699646,-3.79669925955763,-1.93648425285867));
#8833=CARTESIAN_POINT('Ctrl Pts',(82.2476378156836,-1.57031337642494,-4.4148839432415));
#8834=CARTESIAN_POINT('Ctrl Pts',(82.4151271227027,2.84560838224604,-3.72284800486962));
#8835=CARTESIAN_POINT('Ctrl Pts',(82.5826164297219,4.67224268670378,0.3566968026402));
#8836=CARTESIAN_POINT('Ctrl Pts',(82.7501057367407,2.24749108465355,4.11167461709625));
#8837=CARTESIAN_POINT('Ctrl Pts',(82.9175950437602,-2.22230666825049,4.1253408834568));
#8838=CARTESIAN_POINT('Ctrl Pts',(83.0338760378059,-3.92162237958999,1.52875551670549));
#8839=CARTESIAN_POINT('Ctrl Pts',(83.0943272628455,-3.97472621483892,0.110364270143812));
#8840=CARTESIAN_POINT('Ctrl Pts',(83.0989487188788,-3.97408812184296,0.00188072730875047));
#8841=CARTESIAN_POINT('Ctrl Pts',(81.8736667307631,-3.97520616141411,-0.000140328321074999));
#8842=CARTESIAN_POINT('Ctrl Pts',(81.873991386697,-3.97521012478093,-0.00775555150819479));
#8843=CARTESIAN_POINT('Ctrl Pts',(81.9301458116374,-3.97175020506519,-1.32492622653714));
#8844=CARTESIAN_POINT('Ctrl Pts',(82.0421300055841,-2.53120077593259,-3.94336246418788));
#8845=CARTESIAN_POINT('Ctrl Pts',(82.2096193126032,1.92655929036014,-4.27146979303078));
#8846=CARTESIAN_POINT('Ctrl Pts',(82.3771086196222,4.63129675823398,-0.712864102910859));
#8847=CARTESIAN_POINT('Ctrl Pts',(82.5445979266413,3.12190600394933,3.49439376638532));
#8848=CARTESIAN_POINT('Ctrl Pts',(82.7120872336604,-1.22818205067104,4.52201876847685));
#8849=CARTESIAN_POINT('Ctrl Pts',(82.8412212794788,-3.72046301701938,2.14189278432346));
#8850=CARTESIAN_POINT('Ctrl Pts',(82.9145255562908,-3.96899836789274,0.415628650522889));
#8851=CARTESIAN_POINT('Ctrl Pts',(82.9320000640964,-3.96581480482491,0.00322439829302756));
#8852=CARTESIAN_POINT('Origin',(73.0447820522122,0.,0.));
#8853=CARTESIAN_POINT('',(80.8153333974297,-3.96543075761921,-0.00310776878558905));
#8854=CARTESIAN_POINT('',(80.9822820522122,-3.96269713818528,0.00115225484714665));
#8855=CARTESIAN_POINT('',(73.0447820522122,-3.96875,-4.10839266763092E-13));
#8856=CARTESIAN_POINT('Ctrl Pts',(80.9822820522122,-3.96269713818528,0.00115225484714682));
#8857=CARTESIAN_POINT('Ctrl Pts',(81.0132589236582,-3.96077923108138,-0.731358860291098));
#8858=CARTESIAN_POINT('Ctrl Pts',(81.1000655641105,-3.41562392927438,-2.78673257207323));
#8859=CARTESIAN_POINT('Ctrl Pts',(81.2427019735693,-0.115811021377698,-4.68440734136128));
#8860=CARTESIAN_POINT('Ctrl Pts',(81.4101912805881,3.86433888996382,-2.65027720738482));
#8861=CARTESIAN_POINT('Ctrl Pts',(81.5776805876074,4.32823397543431,1.79540385049343));
#8862=CARTESIAN_POINT('Ctrl Pts',(81.7451698946263,0.853764948185291,4.60740379668648));
#8863=CARTESIAN_POINT('Ctrl Pts',(81.8994814939392,-3.06307956634302,3.3356222962608));
#8864=CARTESIAN_POINT('Ctrl Pts',(81.9979633242455,-3.95956025045237,1.00119542712499));
#8865=CARTESIAN_POINT('Ctrl Pts',(82.0406153855455,-3.96867065624537,-0.00356668729390795));
#8866=CARTESIAN_POINT('Ctrl Pts',(80.8153333974297,-3.9654307576192,-0.00310776878558985));
#8867=CARTESIAN_POINT('Ctrl Pts',(80.8334572171033,-3.96859161685811,-0.430940653862831));
#8868=CARTESIAN_POINT('Ctrl Pts',(80.9074108057833,-3.70811382132026,-2.17295237118825));
#8869=CARTESIAN_POINT('Ctrl Pts',(81.0371941634697,-1.17580558461439,-4.53591954505886));
#8870=CARTESIAN_POINT('Ctrl Pts',(81.2046834704886,3.16210773630061,-3.45805719386958));
#8871=CARTESIAN_POINT('Ctrl Pts',(81.3721727775078,4.62274323446282,0.766374503930213));
#8872=CARTESIAN_POINT('Ctrl Pts',(81.5396620845268,1.87703356730924,4.29346362267612));
#8873=CARTESIAN_POINT('Ctrl Pts',(81.706826735612,-2.56800120527708,3.91456288380908));
#8874=CARTESIAN_POINT('Ctrl Pts',(81.8181616176907,-3.97452856060593,1.30180360625973));
#8875=CARTESIAN_POINT('Ctrl Pts',(81.8736667307631,-3.97520616141411,-0.000140328321074999));
#8876=CARTESIAN_POINT('Origin',(73.0447820522122,0.,0.));
#8877=CARTESIAN_POINT('',(79.7570000640964,-3.96446924306102,0.00271090097985122));
#8878=CARTESIAN_POINT('',(79.9239487188789,-3.97281147716045,0.00265889188302577));
#8879=CARTESIAN_POINT('',(73.0447820522122,-3.96875,-4.10839266763092E-13));
#8880=CARTESIAN_POINT('Ctrl Pts',(79.9239487188789,-3.97281147716045,0.00265889188302577));
#8881=CARTESIAN_POINT('Ctrl Pts',(79.9727247540645,-3.96395783417343,-1.14327265515754));
#8882=CARTESIAN_POINT('Ctrl Pts',(80.0773305582564,-2.8417898791282,-3.61598293165399));
#8883=CARTESIAN_POINT('Ctrl Pts',(80.2377661314547,1.35023293842321,-4.48708762389827));
#8884=CARTESIAN_POINT('Ctrl Pts',(80.4052554384738,4.49795344263644,-1.3135825670034));
#8885=CARTESIAN_POINT('Ctrl Pts',(80.5727447454928,3.55287801213224,3.05518283632336));
#8886=CARTESIAN_POINT('Ctrl Pts',(80.7402340525119,-0.625046506306802,4.64396395307223));
#8887=CARTESIAN_POINT('Ctrl Pts',(80.8767464880851,-3.56671435023439,2.49477603427471));
#8888=CARTESIAN_POINT('Ctrl Pts',(80.9574291546518,-3.96423588456471,0.588849554690602));
#8889=CARTESIAN_POINT('Ctrl Pts',(80.9822820522122,-3.96269713818528,0.00115225484714682));
#8890=CARTESIAN_POINT('Ctrl Pts',(79.7570000640964,-3.96446924306102,0.00271090097985101));
#8891=CARTESIAN_POINT('Ctrl Pts',(79.7929230475096,-3.95909204437552,-0.845809344955338));
#8892=CARTESIAN_POINT('Ctrl Pts',(79.8846757999293,-3.27697553121347,-3.02094864559479));
#8893=CARTESIAN_POINT('Ctrl Pts',(80.032258321355,0.296769156290057,-4.67643164821721));
#8894=CARTESIAN_POINT('Ctrl Pts',(80.1997476283743,4.08252384642615,-2.30001824674852));
#8895=CARTESIAN_POINT('Ctrl Pts',(80.3672369353933,4.15349197522231,2.16923703262104));
#8896=CARTESIAN_POINT('Ctrl Pts',(80.5347262424123,0.445097936809096,4.66465140377808));
#8897=CARTESIAN_POINT('Ctrl Pts',(80.6840917297579,-3.22319533629547,3.10485150926155));
#8898=CARTESIAN_POINT('Ctrl Pts',(80.777627448097,-3.9588547046427,0.88698302764329));
#8899=CARTESIAN_POINT('Ctrl Pts',(80.8153333974297,-3.9654307576192,-0.00310776878558985));
#8900=CARTESIAN_POINT('Origin',(73.0447820522122,0.,0.));
#8901=CARTESIAN_POINT('',(78.6986667307631,-3.97495822072444,0.000899384355832079));
#8902=CARTESIAN_POINT('',(78.8656153855456,-3.97038802851853,-0.00340262987801933));
#8903=CARTESIAN_POINT('',(73.0447820522122,-3.96875,-4.10839266763092E-13));
#8904=CARTESIAN_POINT('Ctrl Pts',(78.8656153855456,-3.97038802851853,-0.00340262987801949));
#8905=CARTESIAN_POINT('Ctrl Pts',(78.8763608154644,-3.97267697458941,-0.256253454012208));
#8906=CARTESIAN_POINT('Ctrl Pts',(78.9429360143896,-3.8357540982908,-1.82036601749888));
#8907=CARTESIAN_POINT('Ctrl Pts',(79.065340982321,-1.76003458552832,-4.34273676176006));
#8908=CARTESIAN_POINT('Ctrl Pts',(79.2328302893404,2.68171410172883,-3.84258946710639));
#8909=CARTESIAN_POINT('Ctrl Pts',(79.4003195963591,4.6833066794353,0.154022332581167));
#8910=CARTESIAN_POINT('Ctrl Pts',(79.5678089033785,2.42344595773958,4.01048550943476));
#8911=CARTESIAN_POINT('Ctrl Pts',(79.7352982103974,-2.04156648246805,4.21771153952704));
#8912=CARTESIAN_POINT('Ctrl Pts',(79.8540114822309,-3.88960149513591,1.64443102927543));
#8913=CARTESIAN_POINT('Ctrl Pts',(79.9168949850581,-3.97409184447069,0.168377488708408));
#8914=CARTESIAN_POINT('Ctrl Pts',(79.9239487188789,-3.97281147716045,0.00265889188302577));
#8915=CARTESIAN_POINT('Ctrl Pts',(78.6986667307631,-3.97495822072444,0.000899384355832027));
#8916=CARTESIAN_POINT('Ctrl Pts',(78.7523888779159,-3.97107011656311,-1.25943406802524));
#8917=CARTESIAN_POINT('Ctrl Pts',(78.8619407940752,-2.64373708770944,-3.83659888994191));
#8918=CARTESIAN_POINT('Ctrl Pts',(79.0273224792406,1.73976819338591,-4.35089548826393));
#8919=CARTESIAN_POINT('Ctrl Pts',(79.1948117862598,4.5960799186112,-0.912761895211113));
#8920=CARTESIAN_POINT('Ctrl Pts',(79.3623010932788,3.2703080678004,3.35591567615466));
#8921=CARTESIAN_POINT('Ctrl Pts',(79.529790400298,-1.03119568640402,4.57096492570699));
#8922=CARTESIAN_POINT('Ctrl Pts',(79.6613567239037,-3.67305432406073,2.25824923837563));
#8923=CARTESIAN_POINT('Ctrl Pts',(79.7370932785032,-3.96744902734265,0.472919914885131));
#8924=CARTESIAN_POINT('Ctrl Pts',(79.7570000640964,-3.96446924306102,0.00271090097985101));
#8925=CARTESIAN_POINT('Origin',(73.0447820522122,0.,0.));
#8926=CARTESIAN_POINT('',(77.6403333974297,-3.96694525050465,-0.00346035837147873));
#8927=CARTESIAN_POINT('',(77.8072820522122,-3.96239275275613,0.000241017124700969));
#8928=CARTESIAN_POINT('',(73.0447820522122,-3.96875,-4.10839266763092E-13));
#8929=CARTESIAN_POINT('Ctrl Pts',(77.8072820522122,-3.96239275275613,0.000241017124700885));
#8930=CARTESIAN_POINT('Ctrl Pts',(77.8358266458707,-3.96202476903025,-0.674883524491887));
#8931=CARTESIAN_POINT('Ctrl Pts',(77.9202010085355,-3.4782887115833,-2.67096469036072));
#8932=CARTESIAN_POINT('Ctrl Pts',(78.0604051402067,-0.318569006102588,-4.67499706960582));
#8933=CARTESIAN_POINT('Ctrl Pts',(78.2278944472258,3.74593845389551,-2.81514290719053));
#8934=CARTESIAN_POINT('Ctrl Pts',(78.3953837542449,4.40192649164485,1.60627754211177));
#8935=CARTESIAN_POINT('Ctrl Pts',(78.5628730612639,1.05249582445596,4.56610740188116));
#8936=CARTESIAN_POINT('Ctrl Pts',(78.7196169383641,-2.97829873546034,3.44779152646148));
#8937=CARTESIAN_POINT('Ctrl Pts',(78.820531046458,-3.96078435313356,1.05747742610126));
#8938=CARTESIAN_POINT('Ctrl Pts',(78.8656153855456,-3.97038802851853,-0.00340262987801949));
#8939=CARTESIAN_POINT('Ctrl Pts',(77.6403333974297,-3.96694525050465,-0.00346035837147901));
#8940=CARTESIAN_POINT('Ctrl Pts',(77.6560249393158,-3.97007923854559,-0.373518795794246));
#8941=CARTESIAN_POINT('Ctrl Pts',(77.7275462502083,-3.75324294587763,-2.05662596994668));
#8942=CARTESIAN_POINT('Ctrl Pts',(77.8548973301072,-1.3711384097138,-4.48074328527017));
#8943=CARTESIAN_POINT('Ctrl Pts',(78.0223866371261,3.00938367803536,-3.59175384599341));
#8944=CARTESIAN_POINT('Ctrl Pts',(78.1898759441454,4.65159553477052,0.565459445670238));
#8945=CARTESIAN_POINT('Ctrl Pts',(78.3573652511643,2.06120867216333,4.20814723864878));
#8946=CARTESIAN_POINT('Ctrl Pts',(78.5248545581835,-2.40472141992828,4.02174090914329));
#8947=CARTESIAN_POINT('Ctrl Pts',(78.6386217180497,-3.95192880893686,1.4094223321187));
#8948=CARTESIAN_POINT('Ctrl Pts',(78.6965591089095,-3.97511075843437,0.050344659121072));
#8949=CARTESIAN_POINT('Ctrl Pts',(78.6986667307631,-3.97495822072444,0.000899384355832027));
#8950=CARTESIAN_POINT('Origin',(73.0447820522122,0.,0.));
#8951=CARTESIAN_POINT('',(76.5820000640964,-3.96340732379332,0.00203673152180062));
#8952=CARTESIAN_POINT('',(76.7489487188789,-3.97125648760866,0.00321799934434852));
#8953=CARTESIAN_POINT('',(73.0447820522122,-3.96875,-4.10839266763092E-13));
#8954=CARTESIAN_POINT('Ctrl Pts',(76.7489487188789,-3.97125648760866,0.00321799934434826));
#8955=CARTESIAN_POINT('Ctrl Pts',(76.7952924762769,-3.96167939898907,-1.08668061945271));
#8956=CARTESIAN_POINT('Ctrl Pts',(76.8974660026814,-2.93279899559863,-3.50547381449112));
#8957=CARTESIAN_POINT('Ctrl Pts',(77.0554692980923,1.15464486915952,-4.54134892492803));
#8958=CARTESIAN_POINT('Ctrl Pts',(77.2229586051112,4.43684649216151,-1.50714376233198));
#8959=CARTESIAN_POINT('Ctrl Pts',(77.3904479121304,3.68185494419516,2.8984536307935));
#8960=CARTESIAN_POINT('Ctrl Pts',(77.5579372191495,-0.423344942904035,4.66667541455828));
#8961=CARTESIAN_POINT('Ctrl Pts',(77.6968819325101,-3.50934901946654,2.61091163483654));
#8962=CARTESIAN_POINT('Ctrl Pts',(77.7799968768643,-3.96274450064246,0.645578334589518));
#8963=CARTESIAN_POINT('Ctrl Pts',(77.8072820522122,-3.96239275275613,0.000241017124700885));
#8964=CARTESIAN_POINT('Ctrl Pts',(76.5820000640964,-3.96340732379332,0.00203673152180048));
#8965=CARTESIAN_POINT('Ctrl Pts',(76.6154907697221,-3.95974885929359,-0.789568373245937));
#8966=CARTESIAN_POINT('Ctrl Pts',(76.7048112443542,-3.34708273705454,-2.90604413054571));
#8967=CARTESIAN_POINT('Ctrl Pts',(76.8499614879926,0.0939792462890116,-4.68487346091533));
#8968=CARTESIAN_POINT('Ctrl Pts',(77.0174507950118,3.9790823597631,-2.47467306941385));
#8969=CARTESIAN_POINT('Ctrl Pts',(77.1849401020308,4.24354045361218,1.98733341519075));
#8970=CARTESIAN_POINT('Ctrl Pts',(77.3524294090499,0.646690153391397,4.64099636386739));
#8971=CARTESIAN_POINT('Ctrl Pts',(77.5042271741829,-3.1464884727734,3.21873680013792));
#8972=CARTESIAN_POINT('Ctrl Pts',(77.6001951703095,-3.95892865629787,0.943131743083547));
#8973=CARTESIAN_POINT('Ctrl Pts',(77.6403333974297,-3.96694525050465,-0.00346035837147901));
#8974=CARTESIAN_POINT('Origin',(73.0447820522122,0.,0.));
#8975=CARTESIAN_POINT('',(75.5236667307631,-3.97344267433394,0.00300565485589988));
#8976=CARTESIAN_POINT('',(75.6906153855455,-3.97203085734017,-0.00290119714995032));
#8977=CARTESIAN_POINT('',(73.0447820522122,-3.96875,-4.10839266763092E-13));
#8978=CARTESIAN_POINT('',(75.342557724821,-1.8872933839096,3.49128919534762));
#8979=CARTESIAN_POINT('Ctrl Pts',(75.342557724821,-1.8872933839096,3.49128919534762));
#8980=CARTESIAN_POINT('Ctrl Pts',(75.3983874938273,-3.04449504617051,2.86573831175296));
#8981=CARTESIAN_POINT('Ctrl Pts',(75.4587571624747,-3.92241670625081,1.52403516311381));
#8982=CARTESIAN_POINT('Ctrl Pts',(75.5191268311221,-3.97408386750059,0.109459130694996));
#8983=CARTESIAN_POINT('Ctrl Pts',(75.5236667307631,-3.97344267433394,0.0030056548558996));
#8984=CARTESIAN_POINT('',(75.3425577248209,1.88433026752062,3.49313140215104));
#8985=CARTESIAN_POINT('Origin',(75.342557724821,0.,0.));
#8986=CARTESIAN_POINT('Ctrl Pts',(75.3425577248209,1.88433026752062,3.49313140215104));
#8987=CARTESIAN_POINT('Ctrl Pts',(75.3552305591811,1.62306428446166,3.63777505635095));
#8988=CARTESIAN_POINT('Ctrl Pts',(75.4237331625476,0.127158115454225,4.25847409842879));
#8989=CARTESIAN_POINT('Ctrl Pts',(75.5397523827892,-2.8894493037692,3.55765941766253));
#8990=CARTESIAN_POINT('Ctrl Pts',(75.6430987686705,-3.9626869925898,1.11374971637242));
#8991=CARTESIAN_POINT('Ctrl Pts',(75.6906153855455,-3.97203085734017,-0.00290119714995075));
#8992=CARTESIAN_POINT('Origin',(93.8044,5.12956166756098E-16,0.));
#8993=CARTESIAN_POINT('',(93.8044,-3.4544,-4.23041990297461E-16));
#8994=CARTESIAN_POINT('Origin',(93.8044,0.,0.));
#8995=CARTESIAN_POINT('Origin',(93.8044,0.,0.));
#8996=CARTESIAN_POINT('Ctrl Pts',(93.8044,3.25944077490413,1.14408268708708));
#8997=CARTESIAN_POINT('Ctrl Pts',(93.8044,3.30370182902396,1.04545417171708));
#8998=CARTESIAN_POINT('Ctrl Pts',(93.8044,3.34284347050657,0.944859526825618));
#8999=CARTESIAN_POINT('Ctrl Pts',(93.8044,3.37701350822368,0.842684008101753));
#9000=CARTESIAN_POINT('Ctrl Pts',(93.8044,3.41201453172657,0.738023669067848));
#9001=CARTESIAN_POINT('Ctrl Pts',(93.8044,3.44179939777699,0.631704043659911));
#9002=CARTESIAN_POINT('Ctrl Pts',(93.8044,3.46648177007704,0.524108164188268));
#9003=CARTESIAN_POINT('Ctrl Pts',(93.8044,3.49162219305062,0.414515541273143));
#9004=CARTESIAN_POINT('Ctrl Pts',(93.8044,3.51146916062601,0.303598127467765));
#9005=CARTESIAN_POINT('Ctrl Pts',(93.8044,3.52609364298277,0.191739006411684));
#9006=CARTESIAN_POINT('Ctrl Pts',(93.8044,3.5286056838143,0.17252501492684));
#9007=CARTESIAN_POINT('Ctrl Pts',(93.8044,3.53096351737855,0.153283203416008));
#9008=CARTESIAN_POINT('Ctrl Pts',(93.8044,3.53316735501456,0.134015475734087));
#9009=CARTESIAN_POINT('Ctrl Pts',(93.8044,3.53530980696597,0.11528443126119));
#9010=CARTESIAN_POINT('Ctrl Pts',(93.8044,3.5373057763528,0.0965369355126364));
#9011=CARTESIAN_POINT('Ctrl Pts',(93.8044,3.539155377505,0.0777797908629161));
#9012=CARTESIAN_POINT('Ctrl Pts',(93.8044,3.55040037324356,-0.0362577741564758));
#9013=CARTESIAN_POINT('Ctrl Pts',(93.8044,3.5562458585282,-0.150707951384351));
#9014=CARTESIAN_POINT('Ctrl Pts',(93.8044,3.55681577918696,-0.265159368763883));
#9015=CARTESIAN_POINT('Ctrl Pts',(93.8044,3.55739270972121,-0.381018508731895));
#9016=CARTESIAN_POINT('Ctrl Pts',(93.8044,3.55256361134374,-0.496879755034307));
#9017=CARTESIAN_POINT('Ctrl Pts',(93.8044,3.54240581757772,-0.612333394534078));
#9018=CARTESIAN_POINT('Ctrl Pts',(93.8044,3.53584543270908,-0.68689882941604));
#9019=CARTESIAN_POINT('Ctrl Pts',(93.8044,3.52706130454575,-0.761294558717738));
#9020=CARTESIAN_POINT('Ctrl Pts',(93.8044,3.51606280513667,-0.835411364968679));
#9021=CARTESIAN_POINT('Ctrl Pts',(93.8044,3.51139999040036,-0.866833191123442));
#9022=CARTESIAN_POINT('Ctrl Pts',(93.8044,3.50633906785472,-0.898204884631247));
#9023=CARTESIAN_POINT('Ctrl Pts',(93.8044,3.50088026190799,-0.929518090387137));
#9024=CARTESIAN_POINT('Ctrl Pts',(93.8044,3.49775496561313,-0.947445645769051));
#9025=CARTESIAN_POINT('Ctrl Pts',(93.8044,3.4944990202265,-0.965354850221281));
#9026=CARTESIAN_POINT('Ctrl Pts',(93.8044,3.49111569524411,-0.983227940624935));
#9027=CARTESIAN_POINT('Ctrl Pts',(93.8044,3.4690454343486,-1.09981850472082));
#9028=CARTESIAN_POINT('Ctrl Pts',(93.8044,3.44153185396965,-1.21503326772926));
#9029=CARTESIAN_POINT('Ctrl Pts',(93.8044,3.40868809088207,-1.32844742744932));
#9030=CARTESIAN_POINT('Ctrl Pts',(93.8044,3.37588600130194,-1.44171768265341));
#9031=CARTESIAN_POINT('Ctrl Pts',(93.8044,3.33776721958986,-1.55319282835126));
#9032=CARTESIAN_POINT('Ctrl Pts',(93.8044,3.29439245272803,-1.66245456336488));
#9033=CARTESIAN_POINT('Ctrl Pts',(93.8044,3.25093502747342,-1.77192451619872));
#9034=CARTESIAN_POINT('Ctrl Pts',(93.8044,3.20220157692753,-1.87917356251577));
#9035=CARTESIAN_POINT('Ctrl Pts',(93.8044,3.14820100366361,-1.98377184954477));
#9036=CARTESIAN_POINT('Ctrl Pts',(93.8044,3.12120071703165,-2.03607099305928));
#9037=CARTESIAN_POINT('Ctrl Pts',(93.8044,3.09288283468518,-2.08770721520033));
#9038=CARTESIAN_POINT('Ctrl Pts',(93.8044,3.06324357590169,-2.13862478061915));
#9039=CARTESIAN_POINT('Ctrl Pts',(93.8044,3.04731869343744,-2.16598228812578));
#9040=CARTESIAN_POINT('Ctrl Pts',(93.8044,3.03101229920686,-2.19313230536482));
#9041=CARTESIAN_POINT('Ctrl Pts',(93.8044,3.01432341729309,-2.22006596460196));
#9042=CARTESIAN_POINT('Ctrl Pts',(93.8044,3.00471242017603,-2.23557684919071));
#9043=CARTESIAN_POINT('Ctrl Pts',(93.8044,2.9949745652833,-2.25101597516272));
#9044=CARTESIAN_POINT('Ctrl Pts',(93.8044,2.98510962519026,-2.26638162179989));
#9045=CARTESIAN_POINT('Ctrl Pts',(93.8044,2.98022249157794,-2.27399382901528));
#9046=CARTESIAN_POINT('Ctrl Pts',(93.8044,2.97530477836654,-2.28158703606508));
#9047=CARTESIAN_POINT('Ctrl Pts',(93.8044,2.97035813611545,-2.28915855262409));
#9048=CARTESIAN_POINT('Ctrl Pts',(93.8044,2.9087203455497,-2.38350367164438));
#9049=CARTESIAN_POINT('Ctrl Pts',(93.8044,2.84252153743242,-2.47459708052516));
#9050=CARTESIAN_POINT('Ctrl Pts',(93.8044,2.77218312951852,-2.56235147997252));
#9051=CARTESIAN_POINT('Ctrl Pts',(93.8044,2.69908607066416,-2.65354758024516));
#9052=CARTESIAN_POINT('Ctrl Pts',(93.8044,2.62151807644388,-2.74113813397251));
#9053=CARTESIAN_POINT('Ctrl Pts',(93.8044,2.53989902016449,-2.82500568909054));
#9054=CARTESIAN_POINT('Ctrl Pts',(93.8044,2.4567843214,-2.91041008969875));
#9055=CARTESIAN_POINT('Ctrl Pts',(93.8044,2.36946820531788,-2.99195432509609));
#9056=CARTESIAN_POINT('Ctrl Pts',(93.8044,2.27834636313374,-3.06948664813827));
#9057=CARTESIAN_POINT('Ctrl Pts',(93.8044,2.21740536476488,-3.12133916844289));
#9058=CARTESIAN_POINT('Ctrl Pts',(93.8044,2.15476118149509,-3.17139668069635));
#9059=CARTESIAN_POINT('Ctrl Pts',(93.8044,2.09052247727841,-3.21960525239369));
#9060=CARTESIAN_POINT('Ctrl Pts',(93.8044,2.06033097035291,-3.24226276773458));
#9061=CARTESIAN_POINT('Ctrl Pts',(93.8044,2.02978714981905,-3.26451176450614));
#9062=CARTESIAN_POINT('Ctrl Pts',(93.8044,1.99890180904653,-3.28634604859549));
#9063=CARTESIAN_POINT('Ctrl Pts',(93.8044,1.98422286547466,-3.29672327662868));
#9064=CARTESIAN_POINT('Ctrl Pts',(93.8044,1.96946536617489,-3.30700778786405));
#9065=CARTESIAN_POINT('Ctrl Pts',(93.8044,1.95463485827397,-3.31719585920331));
#9066=CARTESIAN_POINT('Ctrl Pts',(93.8044,1.84995490991091,-3.38910754212328));
#9067=CARTESIAN_POINT('Ctrl Pts',(93.8044,1.74200124640053,-3.45597177584477));
#9068=CARTESIAN_POINT('Ctrl Pts',(93.8044,1.63126903045248,-3.51765019114321));
#9069=CARTESIAN_POINT('Ctrl Pts',(93.8044,1.52297675373357,-3.57796954770892));
#9070=CARTESIAN_POINT('Ctrl Pts',(93.8044,1.41202606433326,-3.63332946958868));
#9071=CARTESIAN_POINT('Ctrl Pts',(93.8044,1.298836561106,-3.68356636248008));
#9072=CARTESIAN_POINT('Ctrl Pts',(93.8044,1.18182163951623,-3.73550109065712));
#9073=CARTESIAN_POINT('Ctrl Pts',(93.8044,1.0624133428104,-3.78196146339442));
#9074=CARTESIAN_POINT('Ctrl Pts',(93.8044,0.941040083796187,-3.82272044533804));
#9075=CARTESIAN_POINT('Ctrl Pts',(93.8044,0.819666824781972,-3.86347942728167));
#9076=CARTESIAN_POINT('Ctrl Pts',(93.8044,0.696327677346945,-3.8985376289676));
#9077=CARTESIAN_POINT('Ctrl Pts',(93.8044,0.571428919000175,-3.92761210585552));
#9078=CARTESIAN_POINT('Ctrl Pts',(93.8044,-2.97061198327651,-2.63181325464289));
#9079=CARTESIAN_POINT('Ctrl Pts',(93.8044,-3.04430299923343,-2.53520263969804));
#9080=CARTESIAN_POINT('Ctrl Pts',(93.8044,-3.11302395750424,-2.43516079500702));
#9081=CARTESIAN_POINT('Ctrl Pts',(93.8044,-3.17676704501544,-2.33211195540638));
#9082=CARTESIAN_POINT('Ctrl Pts',(93.8044,-3.24169167615227,-2.22715299967689));
#9083=CARTESIAN_POINT('Ctrl Pts',(93.8044,-3.30145240555427,-2.11907371594739));
#9084=CARTESIAN_POINT('Ctrl Pts',(93.8044,-3.3559920719374,-2.00829996844531));
#9085=CARTESIAN_POINT('Ctrl Pts',(93.8044,-3.41270540168603,-1.89311136378014));
#9086=CARTESIAN_POINT('Ctrl Pts',(93.8044,-3.46377367315599,-1.7750082788633));
#9087=CARTESIAN_POINT('Ctrl Pts',(93.8044,-3.50907466073431,-1.6544593061801));
#9088=CARTESIAN_POINT('Ctrl Pts',(93.8044,-3.51614057890727,-1.63565642301245));
#9089=CARTESIAN_POINT('Ctrl Pts',(93.8044,-3.52306606694267,-1.61679403209505));
#9090=CARTESIAN_POINT('Ctrl Pts',(93.8044,-3.52985052887756,-1.5978739149434));
#9091=CARTESIAN_POINT('Ctrl Pts',(93.8044,-3.53663923027215,-1.57894197503045));
#9092=CARTESIAN_POINT('Ctrl Pts',(93.8044,-3.54328414598354,-1.55995934744993));
#9093=CARTESIAN_POINT('Ctrl Pts',(93.8044,-3.5497830310177,-1.54093389587887));
#9094=CARTESIAN_POINT('Ctrl Pts',(93.8044,-3.58935229555709,-1.42509508318412));
#9095=CARTESIAN_POINT('Ctrl Pts',(93.8044,-3.62353728821377,-1.30759982045371));
#9096=CARTESIAN_POINT('Ctrl Pts',(93.8044,-3.65228644268449,-1.18886601820872));
#9097=CARTESIAN_POINT('Ctrl Pts',(93.8044,-3.68089336281439,-1.07071964277349));
#9098=CARTESIAN_POINT('Ctrl Pts',(93.8044,-3.70411811636173,-0.951346066625019));
#9099=CARTESIAN_POINT('Ctrl Pts',(93.8044,-3.72185879396385,-0.831153747601256));
#9100=CARTESIAN_POINT('Ctrl Pts',(93.8044,-3.73309728149118,-0.755013483484906));
#9101=CARTESIAN_POINT('Ctrl Pts',(93.8044,-3.74213395530222,-0.678544631812329));
#9102=CARTESIAN_POINT('Ctrl Pts',(93.8044,-3.74893214499955,-0.601852766463008));
#9103=CARTESIAN_POINT('Ctrl Pts',(93.8044,-3.75249425141003,-0.561667864694248));
#9104=CARTESIAN_POINT('Ctrl Pts',(93.8044,-3.75544163433645,-0.521421767935013));
#9105=CARTESIAN_POINT('Ctrl Pts',(93.8044,-3.75776809086273,-0.481129960395163));
#9106=CARTESIAN_POINT('Ctrl Pts',(93.8044,-3.75893451047219,-0.46092878582595));
#9107=CARTESIAN_POINT('Ctrl Pts',(93.8044,-3.75994480481882,-0.440714836914725));
#9108=CARTESIAN_POINT('Ctrl Pts',(93.8044,-3.76079753130694,-0.420510350725053));
#9109=CARTESIAN_POINT('Ctrl Pts',(93.8044,-3.76583949284932,-0.301046203930483));
#9110=CARTESIAN_POINT('Ctrl Pts',(93.8044,-3.76538761743502,-0.181748933042815));
#9111=CARTESIAN_POINT('Ctrl Pts',(93.8044,-3.75937625299169,-0.06300757537429));
#9112=CARTESIAN_POINT('Ctrl Pts',(93.8044,-3.75347847998659,0.0534900318575171));
#9113=CARTESIAN_POINT('Ctrl Pts',(93.8044,-3.74222921402806,0.169453309647518));
#9114=CARTESIAN_POINT('Ctrl Pts',(93.8044,-3.72551718295993,0.284506526530065));
#9115=CARTESIAN_POINT('Ctrl Pts',(93.8044,-3.70832233991097,0.402883640509215));
#9116=CARTESIAN_POINT('Ctrl Pts',(93.8044,-3.68534483519235,0.520298295770664));
#9117=CARTESIAN_POINT('Ctrl Pts',(93.8044,-3.65640891355301,0.6363191991641));
#9118=CARTESIAN_POINT('Ctrl Pts',(93.8044,-3.64194095273334,0.694329650860818));
#9119=CARTESIAN_POINT('Ctrl Pts',(93.8044,-3.62598251867022,0.751991234600619));
#9120=CARTESIAN_POINT('Ctrl Pts',(93.8044,-3.60850639143369,0.809246906377294));
#9121=CARTESIAN_POINT('Ctrl Pts',(93.8044,-3.59937124006994,0.83917568985628));
#9122=CARTESIAN_POINT('Ctrl Pts',(93.8044,-3.58982133903167,0.868993523663466));
#9123=CARTESIAN_POINT('Ctrl Pts',(93.8044,-3.57985241638791,0.898691981790592));
#9124=CARTESIAN_POINT('Ctrl Pts',(93.8044,-3.57385050346129,0.916572305081645));
#9125=CARTESIAN_POINT('Ctrl Pts',(93.8044,-3.56769669888428,0.934409353348099));
#9126=CARTESIAN_POINT('Ctrl Pts',(93.8044,-3.56139002402582,0.952201251079662));
#9127=CARTESIAN_POINT('Ctrl Pts',(93.8044,-3.55813224683699,0.961391837224778));
#9128=CARTESIAN_POINT('Ctrl Pts',(93.8044,-3.55483353387343,0.970570734195694));
#9129=CARTESIAN_POINT('Ctrl Pts',(93.8044,-3.55149565259232,0.979732558860926));
#9130=CARTESIAN_POINT('Ctrl Pts',(93.8044,-3.51235991575605,1.08715242459066));
#9131=CARTESIAN_POINT('Ctrl Pts',(93.8044,-3.46778751151284,1.19238879397286));
#9132=CARTESIAN_POINT('Ctrl Pts',(93.8044,-3.41814899903905,1.29519935184003));
#9133=CARTESIAN_POINT('Ctrl Pts',(93.8044,-3.36777050532375,1.39954254798461));
#9134=CARTESIAN_POINT('Ctrl Pts',(93.8044,-3.31217307851915,1.50138772187045));
#9135=CARTESIAN_POINT('Ctrl Pts',(93.8044,-3.25169578138477,1.60045450315049));
#9136=CARTESIAN_POINT('Ctrl Pts',(93.8044,-3.19103541880398,1.69982116067168));
#9137=CARTESIAN_POINT('Ctrl Pts',(93.8044,-3.12546484916859,1.79639319701438));
#9138=CARTESIAN_POINT('Ctrl Pts',(93.8044,-3.0552887223657,1.88985113911308));
#9139=CARTESIAN_POINT('Ctrl Pts',(93.8044,-3.01248668863769,1.94685328745185));
#9140=CARTESIAN_POINT('Ctrl Pts',(93.8044,-2.96797067855792,2.00269622303262));
#9141=CARTESIAN_POINT('Ctrl Pts',(93.8044,-2.92180480031303,2.05729932119145));
#9142=CARTESIAN_POINT('Ctrl Pts',(93.8044,-2.8974752368903,2.08607532611623));
#9143=CARTESIAN_POINT('Ctrl Pts',(93.8044,-2.87268739712321,2.11450687795852));
#9144=CARTESIAN_POINT('Ctrl Pts',(93.8044,-2.84745035132856,2.14258139753));
#9145=CARTESIAN_POINT('Ctrl Pts',(93.8044,-2.83607676292311,2.15523375125178));
#9146=CARTESIAN_POINT('Ctrl Pts',(93.8044,-2.82461122656622,2.16781425815774));
#9147=CARTESIAN_POINT('Ctrl Pts',(93.8044,-2.8130660969007,2.18030952282467));
#9148=CARTESIAN_POINT('Ctrl Pts',(93.8044,-2.73519313430374,2.26459123348869));
#9149=CARTESIAN_POINT('Ctrl Pts',(93.8044,-2.65358357547324,2.34513111386511));
#9150=CARTESIAN_POINT('Ctrl Pts',(93.8044,-2.56856063424907,2.42166304210725));
#9151=CARTESIAN_POINT('Ctrl Pts',(93.8044,-2.48400757560809,2.49777201367885));
#9152=CARTESIAN_POINT('Ctrl Pts',(93.8044,-2.39607798172114,2.56991771912839));
#9153=CARTESIAN_POINT('Ctrl Pts',(93.8044,-2.30506019564923,2.63779669698566));
#9154=CARTESIAN_POINT('Ctrl Pts',(93.8044,-2.21644895728947,2.70388092674022));
#9155=CARTESIAN_POINT('Ctrl Pts',(93.8044,-2.12490994173969,2.76592135953484));
#9156=CARTESIAN_POINT('Ctrl Pts',(93.8044,-2.03069231632377,2.82359275721866));
#9157=CARTESIAN_POINT('Ctrl Pts',(93.8044,-1.94022059772342,2.87897125396497));
#9158=CARTESIAN_POINT('Ctrl Pts',(93.8044,-1.84727844616327,2.9303213184372));
#9159=CARTESIAN_POINT('Ctrl Pts',(93.8044,-1.75208009336914,2.97731016051328));
#9160=CARTESIAN_POINT('Origin',(73.0447820522122,0.,0.));
#9161=CARTESIAN_POINT('Ctrl Pts',(75.6906153855455,-3.97203085734017,-0.00290119714995075));
#9162=CARTESIAN_POINT('Ctrl Pts',(75.6989285376769,-3.97366559007733,-0.198262094710035));
#9163=CARTESIAN_POINT('Ctrl Pts',(75.7630714588146,-3.87194711440902,-1.70397919582139));
#9164=CARTESIAN_POINT('Ctrl Pts',(75.8830441489587,-1.9464585018686,-4.26281795947025));
#9165=CARTESIAN_POINT('Ctrl Pts',(76.0505334559777,2.51279058774102,-3.9549296545997));
#9166=CARTESIAN_POINT('Ctrl Pts',(76.2180227629969,4.68558178106048,-0.0490381362345196));
#9167=CARTESIAN_POINT('Ctrl Pts',(76.3855120700159,2.59485425351327,3.90182050286693));
#9168=CARTESIAN_POINT('Ctrl Pts',(76.553001377035,-1.85699592939576,4.30214329460675));
#9169=CARTESIAN_POINT('Ctrl Pts',(76.674146926656,-3.85484883176064,1.76030277155817));
#9170=CARTESIAN_POINT('Ctrl Pts',(76.7394627072706,-3.97321680284677,0.22630718179755));
#9171=CARTESIAN_POINT('Ctrl Pts',(76.7489487188789,-3.97125648760866,0.00321799934434826));
#9172=CARTESIAN_POINT('Ctrl Pts',(75.5236667307631,-3.97344267433394,0.0030056548558996));
#9173=CARTESIAN_POINT('Ctrl Pts',(75.5749566001284,-3.96619874465367,-1.19966076974019));
#9174=CARTESIAN_POINT('Ctrl Pts',(75.6820762385001,-2.74440924139197,-3.73144021430678));
#9175=CARTESIAN_POINT('Ctrl Pts',(75.8450256458783,1.55028466462108,-4.42080615645044));
#9176=CARTESIAN_POINT('Ctrl Pts',(76.0125149528972,4.55194904417391,-1.11163115411373));
#9177=CARTESIAN_POINT('Ctrl Pts',(76.1800042599164,3.41272104871659,3.21148763121955));
#9178=CARTESIAN_POINT('Ctrl Pts',(76.3474935669354,-0.83234909652074,4.61115832194601));
#9179=CARTESIAN_POINT('Ctrl Pts',(76.4814921683288,-3.62244148753537,2.37463487493447));
#9180=CARTESIAN_POINT('Ctrl Pts',(76.5596610007158,-3.96584760293371,0.530055364675002));
#9181=CARTESIAN_POINT('Ctrl Pts',(76.5820000640964,-3.96340732379332,0.00203673152180048));
#9182=CARTESIAN_POINT('Ctrl Pts',(75.342557724821,2.66903922910596,-2.1929680694195));
#9183=CARTESIAN_POINT('Ctrl Pts',(75.3983874938273,3.3959072005702,-1.30830442234129));
#9184=CARTESIAN_POINT('Ctrl Pts',(75.5100470318401,3.88844938254442,1.22557529574225));
#9185=CARTESIAN_POINT('Ctrl Pts',(75.6775363388591,1.08737198548797,3.93348015258173));
#9186=CARTESIAN_POINT('Ctrl Pts',(75.8450256458782,-2.70311334847693,3.05287906662549));
#9187=CARTESIAN_POINT('Ctrl Pts',(76.0125149528973,-4.03392091718051,-0.601029078824585));
#9188=CARTESIAN_POINT('Ctrl Pts',(76.1800042599164,-1.69419748002643,-3.71035675192291));
#9189=CARTESIAN_POINT('Ctrl Pts',(76.3474935669354,2.18713292756978,-3.44237077136358));
#9190=CARTESIAN_POINT('Ctrl Pts',(76.5149828739546,4.07833038223504,-0.0426827937785228));
#9191=CARTESIAN_POINT('Ctrl Pts',(76.6824721809735,2.25856114225795,3.39614456569537));
#9192=CARTESIAN_POINT('Ctrl Pts',(76.8499614879927,-1.61632925694607,3.74458552362572));
#9193=CARTESIAN_POINT('Ctrl Pts',(77.0174507950117,-4.02048175693465,0.685815660826552));
#9194=CARTESIAN_POINT('Ctrl Pts',(77.1849401020308,-2.76630182357442,-2.99703369017865));
#9195=CARTESIAN_POINT('Ctrl Pts',(77.3524294090499,1.00500289411644,-3.95279010425736));
#9196=CARTESIAN_POINT('Ctrl Pts',(77.519918716069,3.86183118677738,-1.31181793073376));
#9197=CARTESIAN_POINT('Ctrl Pts',(77.687408023088,3.20468654342747,2.52281404024267));
#9198=CARTESIAN_POINT('Ctrl Pts',(77.8548973301072,-0.36847943830367,4.06187428083153));
#9199=CARTESIAN_POINT('Ctrl Pts',(78.0223866371261,-3.60635710548903,1.90493881793867));
#9200=CARTESIAN_POINT('Ctrl Pts',(78.1898759441453,-3.5627237816556,-1.98534692649581));
#9201=CARTESIAN_POINT('Ctrl Pts',(78.3573652511643,-0.277282462911693,-4.06911744938491));
#9202=CARTESIAN_POINT('Ctrl Pts',(78.5248545581834,3.26046483027065,-2.45030038641864));
#9203=CARTESIAN_POINT('Ctrl Pts',(78.6923438652025,3.83143681832768,1.39810397265408));
#9204=CARTESIAN_POINT('Ctrl Pts',(78.8598331722216,0.916092365606468,3.97433988259736));
#9205=CARTESIAN_POINT('Ctrl Pts',(79.0273224792407,-2.83282654630066,2.93422844240184));
#9206=CARTESIAN_POINT('Ctrl Pts',(79.1948117862598,-4.00408850385809,-0.775807985939492));
#9207=CARTESIAN_POINT('Ctrl Pts',(79.3623010932788,-1.53193410324385,-3.77991807743596));
#9208=CARTESIAN_POINT('Ctrl Pts',(79.5297904002979,2.33416395414478,-3.3445898721694));
#9209=CARTESIAN_POINT('Ctrl Pts',(79.697279707317,4.07635013378049,0.134061038278646));
#9210=CARTESIAN_POINT('Ctrl Pts',(79.8647690143361,2.10936736161653,3.49072658741202));
#9211=CARTESIAN_POINT('Ctrl Pts',(80.0322583213552,-1.77697946634019,3.67109612400433));
#9212=CARTESIAN_POINT('Ctrl Pts',(80.1997476283741,-4.04640997254009,0.51104707139247));
#9213=CARTESIAN_POINT('Ctrl Pts',(80.3672369353934,-2.63391479920022,-3.11401599314157));
#9214=CARTESIAN_POINT('Ctrl Pts',(80.5347262424123,1.17524274960356,-3.90556106784105));
#9215=CARTESIAN_POINT('Ctrl Pts',(80.7022155494315,3.91501867647076,-1.14334226631976));
#9216=CARTESIAN_POINT('Ctrl Pts',(80.8697048564505,3.0924250217599,2.65923114073586));
#9217=CARTESIAN_POINT('Ctrl Pts',(81.0371941634696,-0.544040479089439,4.04210622475407));
#9218=CARTESIAN_POINT('Ctrl Pts',(81.2046834704887,-3.6854704733388,1.74697171277105));
#9219=CARTESIAN_POINT('Ctrl Pts',(81.3721727775078,-3.47340231266724,-2.13777434483456));
#9220=CARTESIAN_POINT('Ctrl Pts',(81.5396620845269,-0.100801913007151,-4.07730814992086));
#9221=CARTESIAN_POINT('Ctrl Pts',(81.7071513915459,3.36352056982451,-2.30680128130774));
#9222=CARTESIAN_POINT('Ctrl Pts',(81.874640698565,3.76729485221803,1.56271951146948));
#9223=CARTESIAN_POINT('Ctrl Pts',(82.0421300055841,0.743117010900478,4.01028426463592));
#9224=CARTESIAN_POINT('Ctrl Pts',(82.2096193126031,-2.9572408576274,2.80879498807853));
#9225=CARTESIAN_POINT('Ctrl Pts',(82.3771086196223,-3.96673419978018,-0.948484350619567));
#9226=CARTESIAN_POINT('Ctrl Pts',(82.5445979266412,-1.36680076284027,-3.8427149841974));
#9227=CARTESIAN_POINT('Ctrl Pts',(82.7120872336604,2.47681753590696,-3.24036690343852));
#9228=CARTESIAN_POINT('Ctrl Pts',(82.8795765406795,4.06672003450697,0.310468897018032));
#9229=CARTESIAN_POINT('Ctrl Pts',(83.0470658476984,1.95621624008245,3.57880158672057));
#9230=CARTESIAN_POINT('Ctrl Pts',(83.2145551547178,-1.93429572404523,3.5906967049608));
#9231=CARTESIAN_POINT('Ctrl Pts',(83.3820444617366,-4.06474552281777,0.335330597781985));
#9232=CARTESIAN_POINT('Ctrl Pts',(83.5495337687559,-2.49658568420434,-3.22516087916586));
#9233=CARTESIAN_POINT('Ctrl Pts',(83.7170230757748,1.343277467771,-3.85100096334118));
#9234=CARTESIAN_POINT('Ctrl Pts',(83.8845123827939,3.96086016944716,-0.9727227216237));
#9235=CARTESIAN_POINT('Ctrl Pts',(84.052001689813,2.97436101339852,2.79065930150043));
#9236=CARTESIAN_POINT('Ctrl Pts',(84.219490996832,-0.718580710202222,4.0147533595479));
#9237=CARTESIAN_POINT('Ctrl Pts',(84.3869803038512,-3.75766857626771,1.5857268510075));
#9238=CARTESIAN_POINT('Ctrl Pts',(84.5544696108703,-3.37756349845322,-2.28619062831437));
#9239=CARTESIAN_POINT('Ctrl Pts',(84.7219589178894,0.0758677780459848,-4.07784831195696));
#9240=CARTESIAN_POINT('Ctrl Pts',(84.8894482249084,3.46026514000546,-2.15897381548248));
#9241=CARTESIAN_POINT('Ctrl Pts',(85.0569375319275,3.69608409210104,1.72440284133193));
#9242=CARTESIAN_POINT('Ctrl Pts',(85.2244268389465,0.568747302491688,4.0387039110319));
#9243=CARTESIAN_POINT('Ctrl Pts',(85.3919161459657,-3.0761063260992,2.67809123175602));
#9244=CARTESIAN_POINT('Ctrl Pts',(85.5594054529847,-3.92193688191295,-1.11938102063903));
#9245=CARTESIAN_POINT('Ctrl Pts',(85.7268947600039,-1.19910281475489,-3.89830158078141));
#9246=CARTESIAN_POINT('Ctrl Pts',(85.8943840670228,2.61482372103935,-3.13006384646798));
#9247=CARTESIAN_POINT('Ctrl Pts',(86.061873374042,4.04945931219474,0.486294205142611));
#9248=CARTESIAN_POINT('Ctrl Pts',(86.229362681061,1.79939455637655,3.66016147260723));
#9249=CARTESIAN_POINT('Ctrl Pts',(86.3968519880802,-2.08798255031681,3.50355985315628));
#9250=CARTESIAN_POINT('Ctrl Pts',(86.5643412950992,-4.07545415494521,0.158984923863421));
#9251=CARTESIAN_POINT('Ctrl Pts',(86.7318306021182,-2.35457208045918,-3.33025420846489));
#9252=CARTESIAN_POINT('Ctrl Pts',(86.8993199091373,1.50879171639289,-3.78921500203144));
#9253=CARTESIAN_POINT('Ctrl Pts',(87.0668092161565,3.99926967039633,-0.800278000774745));
#9254=CARTESIAN_POINT('Ctrl Pts',(87.2342985231755,2.85071603868332,2.91685118610285));
#9255=CARTESIAN_POINT('Ctrl Pts',(87.4017878301946,-0.891772626585205,3.9798673793921));
#9256=CARTESIAN_POINT('Ctrl Pts',(87.5692771372136,-3.8228159473593,1.42150659783601));
#9257=CARTESIAN_POINT('Ctrl Pts',(87.7367664442328,-3.27538716564014,-2.43031719951029));
#9258=CARTESIAN_POINT('Ctrl Pts',(87.9042557512518,0.252395113979941,-4.07073697031827));
#9259=CARTESIAN_POINT('Ctrl Pts',(88.0717450582709,3.55051701369304,-2.00709534166942));
#9260=CARTESIAN_POINT('Ctrl Pts',(88.23923436529,3.6179381546919,1.88285057396995));
#9261=CARTESIAN_POINT('Ctrl Pts',(88.406723672309,0.393310420479956,4.05954550266719));
#9262=CARTESIAN_POINT('Ctrl Pts',(88.5742129793281,-3.18919991757636,2.54236241727983));
#9263=CARTESIAN_POINT('Ctrl Pts',(88.7417022863473,-3.86978060604414,-1.2881773310196));
#9264=CARTESIAN_POINT('Ctrl Pts',(88.9091915933662,-1.02915492040045,-3.94657356765929));
#9265=CARTESIAN_POINT('Ctrl Pts',(89.0766809003854,2.74792356052482,-3.01388766885894));
#9266=CARTESIAN_POINT('Ctrl Pts',(89.2441702074045,4.02460035413828,0.661207051172942));
#9267=CARTESIAN_POINT('Ctrl Pts',(89.4116595144235,1.63919656413269,3.73465358495402));
#9268=CARTESIAN_POINT('Ctrl Pts',(89.5791488214426,-2.23775157363024,3.40984906836557));
#9269=CARTESIAN_POINT('Ctrl Pts',(89.7466381284617,-4.07851577570426,-0.0176590624915208));
#9270=CARTESIAN_POINT('Ctrl Pts',(89.9141274354808,-2.20814045631811,-3.42909878875167));
#9271=CARTESIAN_POINT('Ctrl Pts',(90.0816167424998,1.67147493142775,-3.72031911566969));
#9272=CARTESIAN_POINT('Ctrl Pts',(90.2491060495189,4.03017510942306,-0.626331673446937));
#9273=CARTESIAN_POINT('Ctrl Pts',(90.4165953565381,2.72172209969999,3.03757001658075));
#9274=CARTESIAN_POINT('Ctrl Pts',(90.584084663557,-1.06329125786327,3.93751373657007));
#9275=CARTESIAN_POINT('Ctrl Pts',(90.7515739705761,-3.88079034745029,1.25461910168971));
#9276=CARTESIAN_POINT('Ctrl Pts',(90.9190632775953,-3.16706503236784,-2.5698836498698));
#9277=CARTESIAN_POINT('Ctrl Pts',(91.0865525846142,0.428448863837588,-4.05598742012391));
#9278=CARTESIAN_POINT('Ctrl Pts',(91.2540418916334,3.63410685090686,-1.85145093348772));
#9279=CARTESIAN_POINT('Ctrl Pts',(91.4215311986524,3.53300366018645,2.03776559238545));
#9280=CARTESIAN_POINT('Ctrl Pts',(91.5890205056715,0.217135566134788,4.07276956328891));
#9281=CARTESIAN_POINT('Ctrl Pts',(91.7565098126906,-3.29630946515284,2.401863949772));
#9282=CARTESIAN_POINT('Ctrl Pts',(91.9239991197097,-3.81036316275665,-1.45455799694203));
#9283=CARTESIAN_POINT('Ctrl Pts',(92.0914884267288,-0.85727610730619,-3.98743753572885));
#9284=CARTESIAN_POINT('Ctrl Pts',(92.2589777337478,2.87586759608463,-2.89206194417883));
#9285=CARTESIAN_POINT('Ctrl Pts',(92.426467040767,3.99218924348707,0.834890245879901));
#9286=CARTESIAN_POINT('Ctrl Pts',(92.593956347786,1.4759239582885,3.80211644744834));
#9287=CARTESIAN_POINT('Ctrl Pts',(92.7614456548051,-2.38332395405469,3.30978296485569));
#9288=CARTESIAN_POINT('Ctrl Pts',(92.9289349618241,-4.07392034251622,-0.194354239414968));
#9289=CARTESIAN_POINT('Ctrl Pts',(93.0964242688434,-2.05757404133894,-3.52134293058862));
#9290=CARTESIAN_POINT('Ctrl Pts',(93.2639135758622,1.8310385540054,-3.64477024538087));
#9291=CARTESIAN_POINT('Ctrl Pts',(93.4314028828815,4.05348565523183,-0.450564049263689));
#9292=CARTESIAN_POINT('Ctrl Pts',(93.5988921899005,2.58768524108504,3.15131360915174));
#9293=CARTESIAN_POINT('Ctrl Pts',(93.7663814969195,-1.23293249244653,3.89031122336608));
#9294=CARTESIAN_POINT('Ctrl Pts',(93.9338708039387,-3.93134593579687,1.0800891348575));
#9295=CARTESIAN_POINT('Ctrl Pts',(94.0455303419513,-3.34489230679012,-1.43371602222286));
#9296=CARTESIAN_POINT('Ctrl Pts',(94.1013601109577,-2.58562067024381,-2.29073025684125));
#9297=CARTESIAN_POINT('Ctrl Pts',(75.2435710211684,2.80150992613879,-2.30181023462966));
#9298=CARTESIAN_POINT('Ctrl Pts',(75.2994007901748,3.56445406530438,-1.37323864918543));
#9299=CARTESIAN_POINT('Ctrl Pts',(75.4110603281875,4.08144227469277,1.28640348137652));
#9300=CARTESIAN_POINT('Ctrl Pts',(75.5785496352065,1.14134081565006,4.12870802780178));
#9301=CARTESIAN_POINT('Ctrl Pts',(75.7460389422257,-2.83727522422854,3.20440063794697));
#9302=CARTESIAN_POINT('Ctrl Pts',(75.9135282492446,-4.23413390387881,-0.630859566192717));
#9303=CARTESIAN_POINT('Ctrl Pts',(76.0810175562638,-1.77828448730715,-3.89451048777202));
#9304=CARTESIAN_POINT('Ctrl Pts',(76.2485068632828,2.29568548096019,-3.61322373244229));
#9305=CARTESIAN_POINT('Ctrl Pts',(76.415996170302,4.28074751517686,-0.0448012412638526));
#9306=CARTESIAN_POINT('Ctrl Pts',(76.583485477321,2.37065884600972,3.56470321141922));
#9307=CARTESIAN_POINT('Ctrl Pts',(76.7509747843401,-1.69655148109597,3.93043811395273));
#9308=CARTESIAN_POINT('Ctrl Pts',(76.9184640913592,-4.22002772648839,0.719854305757281));
#9309=CARTESIAN_POINT('Ctrl Pts',(77.0859533983782,-2.90359989202388,-3.14578352406619));
#9310=CARTESIAN_POINT('Ctrl Pts',(77.2534427053974,1.05488355246413,-4.14897637781425));
#9311=CARTESIAN_POINT('Ctrl Pts',(77.4209320124163,4.05350295523876,-1.3769265412665));
#9312=CARTESIAN_POINT('Ctrl Pts',(77.5884213194355,3.3637426770167,2.64802723709294));
#9313=CARTESIAN_POINT('Ctrl Pts',(77.7559106264545,-0.386767939837125,4.26347465874045));
#9314=CARTESIAN_POINT('Ctrl Pts',(77.9233999334736,-3.78534909418059,1.99948541368194));
#9315=CARTESIAN_POINT('Ctrl Pts',(78.0908892404927,-3.73955014581866,-2.08388436586233));
#9316=CARTESIAN_POINT('Ctrl Pts',(78.2583785475118,-0.291044643975323,-4.27107732279188));
#9317=CARTESIAN_POINT('Ctrl Pts',(78.4258678545309,3.42228937147894,-2.57191456000927));
#9318=CARTESIAN_POINT('Ctrl Pts',(78.59335716155,4.02160004276674,1.46749516247331));
#9319=CARTESIAN_POINT('Ctrl Pts',(78.760846468569,0.961560185222965,4.17159572235863));
#9320=CARTESIAN_POINT('Ctrl Pts',(78.9283357755881,-2.97342639326778,3.07986110406517));
#9321=CARTESIAN_POINT('Ctrl Pts',(79.0958250826072,-4.20282083768928,-0.814313161712223));
#9322=CARTESIAN_POINT('Ctrl Pts',(79.2633143896262,-1.60796759733868,-3.967524305544));
#9323=CARTESIAN_POINT('Ctrl Pts',(79.4308036966454,2.45001400333946,-3.5105897371484));
#9324=CARTESIAN_POINT('Ctrl Pts',(79.5982930036644,4.27866898233209,0.140714803046155));
#9325=CARTESIAN_POINT('Ctrl Pts',(79.7657823106835,2.21406022699088,3.6639795614196));
#9326=CARTESIAN_POINT('Ctrl Pts',(79.9332716177026,-1.86517513838281,3.8533012625119));
#9327=CARTESIAN_POINT('Ctrl Pts',(80.1007609247216,-4.24724282044189,0.536411540009373));
#9328=CARTESIAN_POINT('Ctrl Pts',(80.2682502317408,-2.76464218813111,-3.26857193397764));
#9329=CARTESIAN_POINT('Ctrl Pts',(80.4357395387598,1.23357281254345,-4.09940325319346));
#9330=CARTESIAN_POINT('Ctrl Pts',(80.6032288457789,4.10933026519265,-1.20008903321431));
#9331=CARTESIAN_POINT('Ctrl Pts',(80.770718152798,3.24590935188401,2.79121503926503));
#9332=CARTESIAN_POINT('Ctrl Pts',(80.938207459817,-0.571042488161895,4.24272546752679));
#9333=CARTESIAN_POINT('Ctrl Pts',(81.1056967668361,-3.86838904462584,1.83367802939756));
#9334=CARTESIAN_POINT('Ctrl Pts',(81.2731860738552,-3.64579544215624,-2.24387711562598));
#9335=CARTESIAN_POINT('Ctrl Pts',(81.4406753808743,-0.105804949130666,-4.27967454706767));
#9336=CARTESIAN_POINT('Ctrl Pts',(81.6081646878933,3.53046000987095,-2.42129325666677));
#9337=CARTESIAN_POINT('Ctrl Pts',(81.7756539949125,3.95427455995679,1.6402809578108));
#9338=CARTESIAN_POINT('Ctrl Pts',(81.9431433019315,0.779999656662083,4.20932410865277));
#9339=CARTESIAN_POINT('Ctrl Pts',(82.1106326089506,-3.10401567960523,2.94820209226625));
#9340=CARTESIAN_POINT('Ctrl Pts',(82.2781219159697,-4.16361255160751,-0.995559860668701));
#9341=CARTESIAN_POINT('Ctrl Pts',(82.4456112229887,-1.43463830070183,-4.03343797054543));
#9342=CARTESIAN_POINT('Ctrl Pts',(82.6131005300079,2.59974781801999,-3.40119393724889));
#9343=CARTESIAN_POINT('Ctrl Pts',(82.7805898370269,4.26856091857257,0.325878198892089));
#9344=CARTESIAN_POINT('Ctrl Pts',(82.9480791440459,2.05330785493948,3.75642593017913));
#9345=CARTESIAN_POINT('Ctrl Pts',(83.1155684510651,-2.03029937211365,3.76891143112613));
#9346=CARTESIAN_POINT('Ctrl Pts',(83.2830577580841,-4.26648840722233,0.351973844363078));
#9347=CARTESIAN_POINT('Ctrl Pts',(83.4505470651033,-2.62049710603065,-3.3852332022127));
#9348=CARTESIAN_POINT('Ctrl Pts',(83.6180363721222,1.40994748914934,-4.04213520233054));
#9349=CARTESIAN_POINT('Ctrl Pts',(83.7855256791414,4.15744697932781,-1.02100123905723));
#9350=CARTESIAN_POINT('Ctrl Pts',(83.9530149861604,3.12198554899,2.92916628889107));
#9351=CARTESIAN_POINT('Ctrl Pts',(84.1205042931796,-0.754245561627699,4.21401501526076));
#9352=CARTESIAN_POINT('Ctrl Pts',(84.2879936001986,-3.944170509281,1.66443020574501));
#9353=CARTESIAN_POINT('Ctrl Pts',(84.4554829072177,-3.54519992208969,-2.39965964846967));
#9354=CARTESIAN_POINT('Ctrl Pts',(84.6229722142368,0.0796332743828251,-4.28024151861659));
#9355=CARTESIAN_POINT('Ctrl Pts',(84.7904615212558,3.63200624070426,-2.26612876588327));
#9356=CARTESIAN_POINT('Ctrl Pts',(84.957950828275,3.87952944226047,1.80998901176569));
#9357=CARTESIAN_POINT('Ctrl Pts',(85.125440135294,0.596975569343298,4.23915428896914));
#9358=CARTESIAN_POINT('Ctrl Pts',(85.2929294423131,-3.22878072096074,2.8110112009792));
#9359=CARTESIAN_POINT('Ctrl Pts',(85.4604187493321,-4.11659183744908,-1.17493853453105));
#9360=CARTESIAN_POINT('Ctrl Pts',(85.6279080563513,-1.25861710886957,-4.09178346070989));
#9361=CARTESIAN_POINT('Ctrl Pts',(85.7953973633703,2.74460357484093,-3.2854162800243));
#9362=CARTESIAN_POINT('Ctrl Pts',(85.9628866703894,4.25044350599852,0.510430130765498));
#9363=CARTESIAN_POINT('Ctrl Pts',(86.1303759774084,1.88870274207907,3.84182389863737));
#9364=CARTESIAN_POINT('Ctrl Pts',(86.2978652844277,-2.19161403718915,3.67744977233867));
#9365=CARTESIAN_POINT('Ctrl Pts',(86.4653545914466,-4.27772853395903,0.166875719716936));
#9366=CARTESIAN_POINT('Ctrl Pts',(86.6328438984657,-2.47143503298197,-3.49554256072326));
#9367=CARTESIAN_POINT('Ctrl Pts',(86.8003332054849,1.58367659937562,-3.97728265838227));
#9368=CARTESIAN_POINT('Ctrl Pts',(86.9678225125038,4.19776283418438,-0.839997680960255));
#9369=CARTESIAN_POINT('Ctrl Pts',(87.135311819523,2.99220378325032,3.0616213736484));
#9370=CARTESIAN_POINT('Ctrl Pts',(87.302801126542,-0.936033400331159,4.17739756182517));
#9371=CARTESIAN_POINT('Ctrl Pts',(87.4702904335611,-4.01255129768779,1.49205931500802));
#9372=CARTESIAN_POINT('Ctrl Pts',(87.6377797405801,-3.43795233746419,-2.5509395605154));
#9373=CARTESIAN_POINT('Ctrl Pts',(87.8052690475994,0.264922077357618,-4.2727772243598));
#9374=CARTESIAN_POINT('Ctrl Pts',(87.9727583546182,3.72673752724031,-2.10671220605374));
#9375=CARTESIAN_POINT('Ctrl Pts',(88.1402476616376,3.79750493810491,1.97630087819272));
#9376=CARTESIAN_POINT('Ctrl Pts',(88.3077369686564,0.412831342084664,4.26103029783633));
#9377=CARTESIAN_POINT('Ctrl Pts',(88.4752262756755,-3.34748741348548,2.66854584607865));
#9378=CARTESIAN_POINT('Ctrl Pts',(88.6427155826947,-4.06184692288824,-1.35211260296358));
#9379=CARTESIAN_POINT('Ctrl Pts',(88.8102048897137,-1.08023430064092,-4.14245129987768));
#9380=CARTESIAN_POINT('Ctrl Pts',(88.9776941967327,2.88430947253616,-3.1634740053648));
#9381=CARTESIAN_POINT('Ctrl Pts',(89.145183503752,4.22435073936205,0.694024312903952));
#9382=CARTESIAN_POINT('Ctrl Pts',(89.312672810771,1.72055374654368,3.92001322979548));
#9383=CARTESIAN_POINT('Ctrl Pts',(89.4801621177899,-2.34881644952734,3.57908790080283));
#9384=CARTESIAN_POINT('Ctrl Pts',(89.6476514248092,-4.28094211016017,-0.0185355233137089));
#9385=CARTESIAN_POINT('Ctrl Pts',(89.8151407318281,-2.31773566278978,-3.59929303010515));
#9386=CARTESIAN_POINT('Ctrl Pts',(89.9826300388472,1.7544341651567,-3.90496730707241));
#9387=CARTESIAN_POINT('Ctrl Pts',(90.1501193458664,4.23020218286869,-0.657417988121693));
#9388=CARTESIAN_POINT('Ctrl Pts',(90.3176086528855,2.8568075715601,3.18833176372722));
#9389=CARTESIAN_POINT('Ctrl Pts',(90.4850979599045,-1.11606490485281,4.13294180805425));
#9390=CARTESIAN_POINT('Ctrl Pts',(90.6525872669236,-4.07340310366565,1.31688879975151));
#9391=CARTESIAN_POINT('Ctrl Pts',(90.8200765739427,-3.32425392184198,-2.69743302219789));
#9392=CARTESIAN_POINT('Ctrl Pts',(90.9875658809617,0.449713789064823,-4.25729561928448));
#9393=CARTESIAN_POINT('Ctrl Pts',(91.1550551879808,3.81447612475701,-1.94334279967185));
#9394=CARTESIAN_POINT('Ctrl Pts',(91.3225444949999,3.70835494479128,2.13890469347811));
#9395=CARTESIAN_POINT('Ctrl Pts',(91.4900338020189,0.227912515189272,4.27491069970215));
#9396=CARTESIAN_POINT('Ctrl Pts',(91.6575231090381,-3.45991305993065,2.52107410904377));
#9397=CARTESIAN_POINT('Ctrl Pts',(91.8250124160571,-3.99948045208465,-1.52675113281967));
#9398=CARTESIAN_POINT('Ctrl Pts',(91.9925017230763,-0.899824737632048,-4.18534344283303));
#9399=CARTESIAN_POINT('Ctrl Pts',(92.1599910300952,3.0186036716256,-3.03560178332006));
#9400=CARTESIAN_POINT('Ctrl Pts',(92.3274803371144,4.19033098902778,0.87632781323056));
#9401=CARTESIAN_POINT('Ctrl Pts',(92.4949696441334,1.54917753710061,3.99082443289155));
#9402=CARTESIAN_POINT('Ctrl Pts',(92.6624589511525,-2.50161392971549,3.4740552811261));
#9403=CARTESIAN_POINT('Ctrl Pts',(92.8299482581716,-4.27611859481023,-0.204000497621225));
#9404=CARTESIAN_POINT('Ctrl Pts',(92.9974375651908,-2.15969628236128,-3.69611546574651));
#9405=CARTESIAN_POINT('Ctrl Pts',(93.1649268722097,1.9219173057667,-3.82566876858911));
#9406=CARTESIAN_POINT('Ctrl Pts',(93.3324161792289,4.25466968591429,-0.472926603179349));
#9407=CARTESIAN_POINT('Ctrl Pts',(93.4999054862479,2.71611814827125,3.30772071842949));
#9408=CARTESIAN_POINT('Ctrl Pts',(93.667394793267,-1.29412583306428,4.08339652305521));
#9409=CARTESIAN_POINT('Ctrl Pts',(93.834884100286,-4.1264678848162,1.13369650000667));
#9410=CARTESIAN_POINT('Ctrl Pts',(93.9465436382988,-3.51090718231095,-1.50487472185524));
#9411=CARTESIAN_POINT('Ctrl Pts',(94.0023734073051,-2.71395110792135,-2.40442458944182));
#9412=CARTESIAN_POINT('Ctrl Pts',(75.1445843175159,2.93398062317162,-2.41065239983982));
#9413=CARTESIAN_POINT('Ctrl Pts',(75.2004140865222,3.73300093003856,-1.43817287602958));
#9414=CARTESIAN_POINT('Ctrl Pts',(75.3120736245349,4.27443516684111,1.34723166701079));
#9415=CARTESIAN_POINT('Ctrl Pts',(75.479562931554,1.19530964581214,4.32393590302183));
#9416=CARTESIAN_POINT('Ctrl Pts',(75.6470522385732,-2.97143709998015,3.35592220926846));
#9417=CARTESIAN_POINT('Ctrl Pts',(75.8145415455921,-4.43434689057711,-0.66069005356085));
#9418=CARTESIAN_POINT('Ctrl Pts',(75.9820308526113,-1.86237149458788,-4.07866422362114));
#9419=CARTESIAN_POINT('Ctrl Pts',(76.1495201596303,2.40423803435061,-3.784076693521));
#9420=CARTESIAN_POINT('Ctrl Pts',(76.3170094666494,4.48316464811867,-0.0469196887491872));
#9421=CARTESIAN_POINT('Ctrl Pts',(76.4844987736684,2.4827565497615,3.73326185714308));
#9422=CARTESIAN_POINT('Ctrl Pts',(76.6519880806876,-1.77677370524587,4.11629070427974));
#9423=CARTESIAN_POINT('Ctrl Pts',(76.8194773877066,-4.41957369604213,0.753892950688012));
#9424=CARTESIAN_POINT('Ctrl Pts',(76.9869666947257,-3.04089796047335,-3.29453335795373));
#9425=CARTESIAN_POINT('Ctrl Pts',(77.1544560017448,1.10476421081183,-4.34516265137114));
#9426=CARTESIAN_POINT('Ctrl Pts',(77.3219453087638,4.24517472370013,-1.44203515179924));
#9427=CARTESIAN_POINT('Ctrl Pts',(77.4894346157829,3.52279881060593,2.77324043394322));
#9428=CARTESIAN_POINT('Ctrl Pts',(77.656923922802,-0.405056441370581,4.46507503664936));
#9429=CARTESIAN_POINT('Ctrl Pts',(77.8244132298211,-3.96434108287214,2.09403200942523));
#9430=CARTESIAN_POINT('Ctrl Pts',(77.9919025368402,-3.91637650998171,-2.18242180522885));
#9431=CARTESIAN_POINT('Ctrl Pts',(78.1593918438592,-0.304806825038957,-4.47303719619885));
#9432=CARTESIAN_POINT('Ctrl Pts',(78.3268811508783,3.58411391268723,-2.6935287335999));
#9433=CARTESIAN_POINT('Ctrl Pts',(78.4943704578975,4.21176326720579,1.53688635229255));
#9434=CARTESIAN_POINT('Ctrl Pts',(78.6618597649164,1.00702800483946,4.36885156211989));
#9435=CARTESIAN_POINT('Ctrl Pts',(78.8293490719356,-3.11402624023491,3.2254937657285));
#9436=CARTESIAN_POINT('Ctrl Pts',(78.9968383789546,-4.40155317152047,-0.852818337484957));
#9437=CARTESIAN_POINT('Ctrl Pts',(79.1643276859738,-1.6840010914335,-4.15513053365203));
#9438=CARTESIAN_POINT('Ctrl Pts',(79.3318169929927,2.56586405253415,-3.67658960212739));
#9439=CARTESIAN_POINT('Ctrl Pts',(79.4993063000118,4.4809878308837,0.14736856781366));
#9440=CARTESIAN_POINT('Ctrl Pts',(79.666795607031,2.31875309236523,3.83723253542718));
#9441=CARTESIAN_POINT('Ctrl Pts',(79.83428491405,-1.95337081042543,4.03550640101947));
#9442=CARTESIAN_POINT('Ctrl Pts',(80.0017742210691,-4.4480756683437,0.561776008626277));
#9443=CARTESIAN_POINT('Ctrl Pts',(80.1692635280882,-2.89536957706201,-3.42312787481371));
#9444=CARTESIAN_POINT('Ctrl Pts',(80.3367528351073,1.29190287548333,-4.29324543854586));
#9445=CARTESIAN_POINT('Ctrl Pts',(80.5042421421264,4.30364185391454,-1.25683580010885));
#9446=CARTESIAN_POINT('Ctrl Pts',(80.6717314491455,3.39939368200813,2.92319893779419));
#9447=CARTESIAN_POINT('Ctrl Pts',(80.8392207561645,-0.59804449723435,4.44334471029951));
#9448=CARTESIAN_POINT('Ctrl Pts',(81.0067100631835,-4.05130761591287,1.92038434602406));
#9449=CARTESIAN_POINT('Ctrl Pts',(81.1741993702027,-3.81818857164524,-2.3499798864174));
#9450=CARTESIAN_POINT('Ctrl Pts',(81.3416886772217,-0.110807985254183,-4.48204094421447));
#9451=CARTESIAN_POINT('Ctrl Pts',(81.5091779842408,3.69739944991738,-2.53578523202579));
#9452=CARTESIAN_POINT('Ctrl Pts',(81.6766672912599,4.14125426769555,1.71784240415212));
#9453=CARTESIAN_POINT('Ctrl Pts',(81.8441565982789,0.816882302423688,4.40836395266962));
#9454=CARTESIAN_POINT('Ctrl Pts',(82.0116459052981,-3.25079050158307,3.08760919645398));
#9455=CARTESIAN_POINT('Ctrl Pts',(82.1791352123171,-4.36049090343483,-1.04263537071784));
#9456=CARTESIAN_POINT('Ctrl Pts',(82.3466245193362,-1.50247583856339,-4.22416095689346));
#9457=CARTESIAN_POINT('Ctrl Pts',(82.5141138263553,2.72267810013302,-3.56202097105925));
#9458=CARTESIAN_POINT('Ctrl Pts',(82.6816031333744,4.47040180263817,0.341287500766147));
#9459=CARTESIAN_POINT('Ctrl Pts',(82.8490924403934,2.15039946979652,3.93405027363768));
#9460=CARTESIAN_POINT('Ctrl Pts',(83.0165817474126,-2.12630302018207,3.94712615729146));
#9461=CARTESIAN_POINT('Ctrl Pts',(83.1840710544315,-4.46823129162689,0.368617090944171));
#9462=CARTESIAN_POINT('Ctrl Pts',(83.3515603614508,-2.74440852785697,-3.54530552525954));
#9463=CARTESIAN_POINT('Ctrl Pts',(83.5190496684696,1.47661751052768,-4.2332694413199));
#9464=CARTESIAN_POINT('Ctrl Pts',(83.686538975489,4.35403378920846,-1.06927975649076));
#9465=CARTESIAN_POINT('Ctrl Pts',(83.8540282825078,3.26961008458147,3.06767327628172));
#9466=CARTESIAN_POINT('Ctrl Pts',(84.0215175895271,-0.789910413053178,4.41327667097361));
#9467=CARTESIAN_POINT('Ctrl Pts',(84.1890068965459,-4.13067244229429,1.74313356048251));
#9468=CARTESIAN_POINT('Ctrl Pts',(84.3564962035653,-3.71283634572615,-2.51312866862498));
#9469=CARTESIAN_POINT('Ctrl Pts',(84.523985510584,0.0833987707196642,-4.48263472527622));
#9470=CARTESIAN_POINT('Ctrl Pts',(84.6914748176035,3.80374734140306,-2.37328371628405));
#9471=CARTESIAN_POINT('Ctrl Pts',(84.8589641246222,4.06297479241989,1.89557518219944));
#9472=CARTESIAN_POINT('Ctrl Pts',(85.0264534316416,0.625203836194908,4.43960466690639));
#9473=CARTESIAN_POINT('Ctrl Pts',(85.1939427386604,-3.38145511582228,2.94393117020239));
#9474=CARTESIAN_POINT('Ctrl Pts',(85.3614320456797,-4.3112467929852,-1.23049604842306));
#9475=CARTESIAN_POINT('Ctrl Pts',(85.5289213526986,-1.31813140298424,-4.28526534063838));
#9476=CARTESIAN_POINT('Ctrl Pts',(85.6964106597178,2.87438342864251,-3.44076871358061));
#9477=CARTESIAN_POINT('Ctrl Pts',(85.8638999667368,4.45142769980231,0.534566056388386));
#9478=CARTESIAN_POINT('Ctrl Pts',(86.0313892737559,1.97801092778158,4.02348632466751));
#9479=CARTESIAN_POINT('Ctrl Pts',(86.198878580775,-2.29524552406149,3.85133969152105));
#9480=CARTESIAN_POINT('Ctrl Pts',(86.3663678877941,-4.48000291297286,0.174766515570451));
#9481=CARTESIAN_POINT('Ctrl Pts',(86.5338571948131,-2.58829798550476,-3.66083091298163));
#9482=CARTESIAN_POINT('Ctrl Pts',(86.7013465018322,1.65856148235836,-4.16535031473309));
#9483=CARTESIAN_POINT('Ctrl Pts',(86.8688358088513,4.39625599797244,-0.87971736114577));
#9484=CARTESIAN_POINT('Ctrl Pts',(87.0363251158703,3.13369152781732,3.20639156119395));
#9485=CARTESIAN_POINT('Ctrl Pts',(87.2038144228895,-0.980294174077118,4.37492774425823));
#9486=CARTESIAN_POINT('Ctrl Pts',(87.3713037299086,-4.20228664801629,1.56261203218003));
#9487=CARTESIAN_POINT('Ctrl Pts',(87.5387930369276,-3.60051750928825,-2.67156192152051));
#9488=CARTESIAN_POINT('Ctrl Pts',(87.7062823439467,0.277449040735304,-4.47481747840133));
#9489=CARTESIAN_POINT('Ctrl Pts',(87.8737716509658,3.90295804078757,-2.20632907043807));
#9490=CARTESIAN_POINT('Ctrl Pts',(88.0412609579849,3.97707172151794,2.06975118241549));
#9491=CARTESIAN_POINT('Ctrl Pts',(88.2087502650039,0.432352263689362,4.46251509300548));
#9492=CARTESIAN_POINT('Ctrl Pts',(88.376239572023,-3.50577490939459,2.79472927487746));
#9493=CARTESIAN_POINT('Ctrl Pts',(88.5437288790421,-4.25391323973235,-1.41604787490757));
#9494=CARTESIAN_POINT('Ctrl Pts',(88.7112181860611,-1.13131368088138,-4.33832903209606));
#9495=CARTESIAN_POINT('Ctrl Pts',(88.8787074930802,3.0206953845475,-3.31306034187067));
#9496=CARTESIAN_POINT('Ctrl Pts',(89.0461968000993,4.42410112458583,0.726841574634959));
#9497=CARTESIAN_POINT('Ctrl Pts',(89.2136861071185,1.80191092895468,4.10537287463695));
#9498=CARTESIAN_POINT('Ctrl Pts',(89.3811754141374,-2.45988132542442,3.74832673324009));
#9499=CARTESIAN_POINT('Ctrl Pts',(89.5486647211567,-4.48336844461608,-0.019411984135895));
#9500=CARTESIAN_POINT('Ctrl Pts',(89.7161540281755,-2.42733086926145,-3.76948727145864));
#9501=CARTESIAN_POINT('Ctrl Pts',(89.8836433351947,1.83739339888565,-4.08961549847513));
#9502=CARTESIAN_POINT('Ctrl Pts',(90.0511326422138,4.43022925631431,-0.68850430279645));
#9503=CARTESIAN_POINT('Ctrl Pts',(90.2186219492329,2.99189304342021,3.33909351087369));
#9504=CARTESIAN_POINT('Ctrl Pts',(90.3861112562519,-1.16883855184235,4.32836987953842));
#9505=CARTESIAN_POINT('Ctrl Pts',(90.5536005632711,-4.26601585988102,1.37915849781332));
#9506=CARTESIAN_POINT('Ctrl Pts',(90.72108987029,-3.48144281131612,-2.82498239452599));
#9507=CARTESIAN_POINT('Ctrl Pts',(90.8885791773093,0.470978714292056,-4.45860381844503));
#9508=CARTESIAN_POINT('Ctrl Pts',(91.0560684843282,3.99484539860717,-2.03523466585599));
#9509=CARTESIAN_POINT('Ctrl Pts',(91.2235577913474,3.88370622939613,2.24004379457078));
#9510=CARTESIAN_POINT('Ctrl Pts',(91.3910470983663,0.238689464243757,4.47705183611538));
#9511=CARTESIAN_POINT('Ctrl Pts',(91.5585364053856,-3.62351665470846,2.64028426831555));
#9512=CARTESIAN_POINT('Ctrl Pts',(91.7260257124045,-4.18859774141264,-1.59894426869731));
#9513=CARTESIAN_POINT('Ctrl Pts',(91.8935150194237,-0.942373367957906,-4.38324934993722));
#9514=CARTESIAN_POINT('Ctrl Pts',(92.0610043264428,3.16133974716656,-3.17914162246129));
#9515=CARTESIAN_POINT('Ctrl Pts',(92.2284936334618,4.3884727345685,0.917765380581216));
#9516=CARTESIAN_POINT('Ctrl Pts',(92.3959829404809,1.62243111591272,4.17953241833476));
#9517=CARTESIAN_POINT('Ctrl Pts',(92.5634722475,-2.61990390537629,3.63832759739651));
#9518=CARTESIAN_POINT('Ctrl Pts',(92.7309615545189,-4.47831684710423,-0.213646755827483));
#9519=CARTESIAN_POINT('Ctrl Pts',(92.8984508615383,-2.26181852338362,-3.8708880009044));
#9520=CARTESIAN_POINT('Ctrl Pts',(93.0659401685571,2.012796057528,-4.00656729179735));
#9521=CARTESIAN_POINT('Ctrl Pts',(93.2334294755763,4.45585371659675,-0.495289157095007));
#9522=CARTESIAN_POINT('Ctrl Pts',(93.4009187825954,2.84455105545746,3.46412782770724));
#9523=CARTESIAN_POINT('Ctrl Pts',(93.5684080896144,-1.35531917368203,4.27648182274434));
#9524=CARTESIAN_POINT('Ctrl Pts',(93.7358973966335,-4.32158983383552,1.18730386515585));
#9525=CARTESIAN_POINT('Ctrl Pts',(93.8475569346462,-3.67692205783178,-1.57603342148763));
#9526=CARTESIAN_POINT('Ctrl Pts',(93.9033867036526,-2.84228154559889,-2.5181189220424));
#9527=CARTESIAN_POINT('Ctrl Pts',(75.0455976138633,3.06645132020445,-2.51949456504998));
#9528=CARTESIAN_POINT('Ctrl Pts',(75.1014273828696,3.90154779477274,-1.50310710287372));
#9529=CARTESIAN_POINT('Ctrl Pts',(75.2130869208824,4.46742805898946,1.40805985264505));
#9530=CARTESIAN_POINT('Ctrl Pts',(75.3805762279014,1.24927847597423,4.51916377824188));
#9531=CARTESIAN_POINT('Ctrl Pts',(75.5480655349206,-3.10559897573176,3.50744378058995));
#9532=CARTESIAN_POINT('Ctrl Pts',(75.7155548419395,-4.63455987727541,-0.69052054092898));
#9533=CARTESIAN_POINT('Ctrl Pts',(75.8830441489587,-1.9464585018686,-4.26281795947025));
#9534=CARTESIAN_POINT('Ctrl Pts',(76.0505334559777,2.51279058774102,-3.9549296545997));
#9535=CARTESIAN_POINT('Ctrl Pts',(76.2180227629969,4.68558178106048,-0.0490381362345196));
#9536=CARTESIAN_POINT('Ctrl Pts',(76.3855120700159,2.59485425351327,3.90182050286693));
#9537=CARTESIAN_POINT('Ctrl Pts',(76.553001377035,-1.85699592939576,4.30214329460675));
#9538=CARTESIAN_POINT('Ctrl Pts',(76.720490684054,-4.61911966559588,0.787931595618742));
#9539=CARTESIAN_POINT('Ctrl Pts',(76.8879799910731,-3.17819602892282,-3.44328319184127));
#9540=CARTESIAN_POINT('Ctrl Pts',(77.0554692980923,1.15464486915952,-4.54134892492803));
#9541=CARTESIAN_POINT('Ctrl Pts',(77.2229586051112,4.43684649216151,-1.50714376233198));
#9542=CARTESIAN_POINT('Ctrl Pts',(77.3904479121304,3.68185494419516,2.8984536307935));
#9543=CARTESIAN_POINT('Ctrl Pts',(77.5579372191495,-0.423344942904035,4.66667541455828));
#9544=CARTESIAN_POINT('Ctrl Pts',(77.7254265261685,-4.14333307156369,2.18857860516851));
#9545=CARTESIAN_POINT('Ctrl Pts',(77.8929158331877,-4.09320287414477,-2.28095924459537));
#9546=CARTESIAN_POINT('Ctrl Pts',(78.0604051402067,-0.318569006102588,-4.67499706960582));
#9547=CARTESIAN_POINT('Ctrl Pts',(78.2278944472258,3.74593845389551,-2.81514290719053));
#9548=CARTESIAN_POINT('Ctrl Pts',(78.3953837542449,4.40192649164485,1.60627754211177));
#9549=CARTESIAN_POINT('Ctrl Pts',(78.5628730612639,1.05249582445596,4.56610740188116));
#9550=CARTESIAN_POINT('Ctrl Pts',(78.7303623682829,-3.25462608720204,3.37112642739182));
#9551=CARTESIAN_POINT('Ctrl Pts',(78.8978516753021,-4.60028550535166,-0.891323513257688));
#9552=CARTESIAN_POINT('Ctrl Pts',(79.065340982321,-1.76003458552832,-4.34273676176006));
#9553=CARTESIAN_POINT('Ctrl Pts',(79.2328302893404,2.68171410172883,-3.84258946710639));
#9554=CARTESIAN_POINT('Ctrl Pts',(79.4003195963591,4.6833066794353,0.154022332581167));
#9555=CARTESIAN_POINT('Ctrl Pts',(79.5678089033785,2.42344595773958,4.01048550943476));
#9556=CARTESIAN_POINT('Ctrl Pts',(79.7352982103974,-2.04156648246805,4.21771153952704));
#9557=CARTESIAN_POINT('Ctrl Pts',(79.9027875174165,-4.64890851624551,0.58714047724318));
#9558=CARTESIAN_POINT('Ctrl Pts',(80.0702768244356,-3.0260969659929,-3.57768381564977));
#9559=CARTESIAN_POINT('Ctrl Pts',(80.2377661314547,1.35023293842321,-4.48708762389827));
#9560=CARTESIAN_POINT('Ctrl Pts',(80.4052554384738,4.49795344263644,-1.3135825670034));
#9561=CARTESIAN_POINT('Ctrl Pts',(80.5727447454928,3.55287801213224,3.05518283632336));
#9562=CARTESIAN_POINT('Ctrl Pts',(80.7402340525119,-0.625046506306802,4.64396395307223));
#9563=CARTESIAN_POINT('Ctrl Pts',(80.907723359531,-4.23422618719991,2.00709066265056));
#9564=CARTESIAN_POINT('Ctrl Pts',(81.07521266655,-3.99058170113424,-2.45608265720882));
#9565=CARTESIAN_POINT('Ctrl Pts',(81.2427019735693,-0.115811021377698,-4.68440734136128));
#9566=CARTESIAN_POINT('Ctrl Pts',(81.4101912805881,3.86433888996382,-2.65027720738482));
#9567=CARTESIAN_POINT('Ctrl Pts',(81.5776805876074,4.32823397543431,1.79540385049343));
#9568=CARTESIAN_POINT('Ctrl Pts',(81.7451698946263,0.853764948185291,4.60740379668648));
#9569=CARTESIAN_POINT('Ctrl Pts',(81.9126592016455,-3.39756532356089,3.2270163006417));
#9570=CARTESIAN_POINT('Ctrl Pts',(82.0801485086645,-4.55736925526216,-1.08971088076697));
#9571=CARTESIAN_POINT('Ctrl Pts',(82.2476378156836,-1.57031337642494,-4.4148839432415));
#9572=CARTESIAN_POINT('Ctrl Pts',(82.4151271227027,2.84560838224604,-3.72284800486962));
#9573=CARTESIAN_POINT('Ctrl Pts',(82.5826164297219,4.67224268670378,0.3566968026402));
#9574=CARTESIAN_POINT('Ctrl Pts',(82.7501057367407,2.24749108465355,4.11167461709625));
#9575=CARTESIAN_POINT('Ctrl Pts',(82.9175950437602,-2.22230666825049,4.1253408834568));
#9576=CARTESIAN_POINT('Ctrl Pts',(83.0850843507788,-4.66997417603144,0.385260337525263));
#9577=CARTESIAN_POINT('Ctrl Pts',(83.2525736577983,-2.86831994968329,-3.70537784830637));
#9578=CARTESIAN_POINT('Ctrl Pts',(83.4200629648169,1.54328753190602,-4.42440368030926));
#9579=CARTESIAN_POINT('Ctrl Pts',(83.5875522718364,4.5506205990891,-1.11755827392429));
#9580=CARTESIAN_POINT('Ctrl Pts',(83.7550415788553,3.41723462017294,3.20618026367237));
#9581=CARTESIAN_POINT('Ctrl Pts',(83.9225308858744,-0.825575264478656,4.61253832668647));
#9582=CARTESIAN_POINT('Ctrl Pts',(84.0900201928935,-4.31717437530757,1.82183691522002));
#9583=CARTESIAN_POINT('Ctrl Pts',(84.2575094999126,-3.88047276936262,-2.62659768878029));
#9584=CARTESIAN_POINT('Ctrl Pts',(84.4249988069316,0.0871642670565068,-4.68502793193585));
#9585=CARTESIAN_POINT('Ctrl Pts',(84.5924881139508,3.97548844210186,-2.48043866668484));
#9586=CARTESIAN_POINT('Ctrl Pts',(84.7599774209698,4.24642014257932,1.9811613526332));
#9587=CARTESIAN_POINT('Ctrl Pts',(84.9274667279889,0.653432103046516,4.64005504484363));
#9588=CARTESIAN_POINT('Ctrl Pts',(85.0949560350079,-3.53412951068382,3.07685113942557));
#9589=CARTESIAN_POINT('Ctrl Pts',(85.262445342027,-4.50590174852132,-1.28605356231507));
#9590=CARTESIAN_POINT('Ctrl Pts',(85.4299346490461,-1.37764569709891,-4.47874722056687));
#9591=CARTESIAN_POINT('Ctrl Pts',(85.5974239560652,3.0041632824441,-3.59612114713693));
#9592=CARTESIAN_POINT('Ctrl Pts',(85.7649132630843,4.65241189360609,0.558701982011273));
#9593=CARTESIAN_POINT('Ctrl Pts',(85.9324025701033,2.06731911348409,4.20514875069765));
#9594=CARTESIAN_POINT('Ctrl Pts',(86.0998918771224,-2.39887701093383,4.02522961070344));
#9595=CARTESIAN_POINT('Ctrl Pts',(86.2673811841415,-4.68227729198668,0.182657311423967));
#9596=CARTESIAN_POINT('Ctrl Pts',(86.4348704911605,-2.70516093802755,-3.82611926523999));
#9597=CARTESIAN_POINT('Ctrl Pts',(86.6023597981797,1.7334463653411,-4.35341797108391));
#9598=CARTESIAN_POINT('Ctrl Pts',(86.7698491051987,4.59474916176048,-0.919437041331279));
#9599=CARTESIAN_POINT('Ctrl Pts',(86.9373384122179,3.27517927238433,3.35116174873949));
#9600=CARTESIAN_POINT('Ctrl Pts',(87.1048277192368,-1.02455494782308,4.5724579266913));
#9601=CARTESIAN_POINT('Ctrl Pts',(87.2723170262561,-4.39202199834478,1.63316474935204));
#9602=CARTESIAN_POINT('Ctrl Pts',(87.439806333275,-3.7630826811123,-2.79218428252561));
#9603=CARTESIAN_POINT('Ctrl Pts',(87.6072956402942,0.289976004112983,-4.67685773244287));
#9604=CARTESIAN_POINT('Ctrl Pts',(87.7747849473131,4.07917855433484,-2.3059459348224));
#9605=CARTESIAN_POINT('Ctrl Pts',(87.9422742543323,4.15663850493095,2.16320148663827));
#9606=CARTESIAN_POINT('Ctrl Pts',(88.1097635613514,0.451873185294068,4.66399988817462));
#9607=CARTESIAN_POINT('Ctrl Pts',(88.2772528683704,-3.66406240530372,2.92091270367628));
#9608=CARTESIAN_POINT('Ctrl Pts',(88.4447421753896,-4.44597955657645,-1.47998314685156));
#9609=CARTESIAN_POINT('Ctrl Pts',(88.6122314824085,-1.18239306112185,-4.53420676431444));
#9610=CARTESIAN_POINT('Ctrl Pts',(88.7797207894278,3.15708129655885,-3.46264667837653));
#9611=CARTESIAN_POINT('Ctrl Pts',(88.9472100964467,4.6238515098096,0.75965883636597));
#9612=CARTESIAN_POINT('Ctrl Pts',(89.1146994034659,1.88326811136568,4.29073251947842));
#9613=CARTESIAN_POINT('Ctrl Pts',(89.2821887104849,-2.57094620132151,3.91756556567735));
#9614=CARTESIAN_POINT('Ctrl Pts',(89.4496780175041,-4.68579477907199,-0.0202884449580863));
#9615=CARTESIAN_POINT('Ctrl Pts',(89.617167324523,-2.53692607573313,-3.93968151281212));
#9616=CARTESIAN_POINT('Ctrl Pts',(89.7846566315422,1.9203526326146,-4.27426368987786));
#9617=CARTESIAN_POINT('Ctrl Pts',(89.9521459385612,4.63025632975995,-0.719590617471205));
#9618=CARTESIAN_POINT('Ctrl Pts',(90.1196352455803,3.12697851528032,3.48985525802016));
#9619=CARTESIAN_POINT('Ctrl Pts',(90.2871245525994,-1.22161219883188,4.5237979510226));
#9620=CARTESIAN_POINT('Ctrl Pts',(90.4546138596185,-4.45862861609638,1.44142819587512));
#9621=CARTESIAN_POINT('Ctrl Pts',(90.6221031666375,-3.63863170079026,-2.95253176685409));
#9622=CARTESIAN_POINT('Ctrl Pts',(90.7895924736566,0.492243639519289,-4.6599120176056));
#9623=CARTESIAN_POINT('Ctrl Pts',(90.9570817806758,4.17521467245732,-2.12712653204012));
#9624=CARTESIAN_POINT('Ctrl Pts',(91.1245710876947,4.05905751400097,2.34118289566344));
#9625=CARTESIAN_POINT('Ctrl Pts',(91.2920603947138,0.249466413298239,4.67919297252862));
#9626=CARTESIAN_POINT('Ctrl Pts',(91.4595497017329,-3.78712024948626,2.75949442758732));
#9627=CARTESIAN_POINT('Ctrl Pts',(91.6270390087521,-4.37771503074064,-1.67113740457495));
#9628=CARTESIAN_POINT('Ctrl Pts',(91.7945283157709,-0.984921998283766,-4.58115525704141));
#9629=CARTESIAN_POINT('Ctrl Pts',(91.9620176227903,3.30407582270753,-3.32268146160252));
#9630=CARTESIAN_POINT('Ctrl Pts',(92.1295069298092,4.58661448010922,0.959202947931876));
#9631=CARTESIAN_POINT('Ctrl Pts',(92.2969962368283,1.69568469472483,4.36824040377796));
#9632=CARTESIAN_POINT('Ctrl Pts',(92.4644855438475,-2.73819388103709,3.80259991366693));
#9633=CARTESIAN_POINT('Ctrl Pts',(92.6319748508664,-4.68051509939824,-0.22329301403374));
#9634=CARTESIAN_POINT('Ctrl Pts',(92.7994641578856,-2.36394076440595,-4.0456605360623));
#9635=CARTESIAN_POINT('Ctrl Pts',(92.9669534649047,2.10367480928929,-4.18746581500559));
#9636=CARTESIAN_POINT('Ctrl Pts',(93.1344427719237,4.65703774727922,-0.51765171101067));
#9637=CARTESIAN_POINT('Ctrl Pts',(93.3019320789428,2.97298396264366,3.62053493698499));
#9638=CARTESIAN_POINT('Ctrl Pts',(93.4694213859619,-1.41651251429978,4.46956712243346));
#9639=CARTESIAN_POINT('Ctrl Pts',(93.6369106929809,-4.51671178285486,1.24091123030503));
#9640=CARTESIAN_POINT('Ctrl Pts',(93.7485702309937,-3.84293693335262,-1.64719212112001));
#9641=CARTESIAN_POINT('Ctrl Pts',(93.8044,-2.97061198327643,-2.63181325464298));
#9642=CARTESIAN_POINT('Ctrl Pts',(75.342557724821,2.66903922910601,-2.19296806941944));
#9643=CARTESIAN_POINT('Ctrl Pts',(75.342557724821,2.74445357713776,-2.11551288776751));
#9644=CARTESIAN_POINT('Ctrl Pts',(75.342557724821,2.81573387113398,-2.03445442488076));
#9645=CARTESIAN_POINT('Ctrl Pts',(75.342557724821,2.88288676332201,-1.95020526406688));
#9646=CARTESIAN_POINT('Ctrl Pts',(75.342557724821,2.95167275371243,-1.8639072391074));
#9647=CARTESIAN_POINT('Ctrl Pts',(75.342557724821,3.01612853799601,-1.77426095588347));
#9648=CARTESIAN_POINT('Ctrl Pts',(75.342557724821,3.07622945879123,-1.68166519380833));
#9649=CARTESIAN_POINT('Ctrl Pts',(75.342557724821,3.13744571756752,-1.58735106254747));
#9650=CARTESIAN_POINT('Ctrl Pts',(75.342557724821,3.19414439702615,-1.48997634213879));
#9651=CARTESIAN_POINT('Ctrl Pts',(75.342557724821,3.24626072027771,-1.38992521171123));
#9652=CARTESIAN_POINT('Ctrl Pts',(75.342557724821,3.25521273849457,-1.37273943408296));
#9653=CARTESIAN_POINT('Ctrl Pts',(75.342557724821,3.2640294549757,-1.35547461535056));
#9654=CARTESIAN_POINT('Ctrl Pts',(75.342557724821,3.27271041500071,-1.33813261632123));
#9655=CARTESIAN_POINT('Ctrl Pts',(75.342557724821,3.28114951999669,-1.32127377234235));
#9656=CARTESIAN_POINT('Ctrl Pts',(75.342557724821,3.28945668002034,-1.30434921737686));
#9657=CARTESIAN_POINT('Ctrl Pts',(75.342557724821,3.29762966865746,-1.28736537979867));
#9658=CARTESIAN_POINT('Ctrl Pts',(75.342557724821,3.34731909381879,-1.18410852190207));
#9659=CARTESIAN_POINT('Ctrl Pts',(75.342557724821,3.39207834736118,-1.07861149239416));
#9660=CARTESIAN_POINT('Ctrl Pts',(75.342557724821,3.43188270629604,-0.971303217913125));
#9661=CARTESIAN_POINT('Ctrl Pts',(75.342557724821,3.47217664595643,-0.862675086404327));
#9662=CARTESIAN_POINT('Ctrl Pts',(75.342557724821,3.50739344417012,-0.752190133416963));
#9663=CARTESIAN_POINT('Ctrl Pts',(75.342557724821,3.53746516435151,-0.640259734304225));
#9664=CARTESIAN_POINT('Ctrl Pts',(75.342557724821,3.5568869054314,-0.567969781570485));
#9665=CARTESIAN_POINT('Ctrl Pts',(75.342557724821,3.57416166527878,-0.495076252130135));
#9666=CARTESIAN_POINT('Ctrl Pts',(75.342557724821,3.58926077368719,-0.421684949048237));
#9667=CARTESIAN_POINT('Ctrl Pts',(75.342557724821,3.59566205252182,-0.390570648630151));
#9668=CARTESIAN_POINT('Ctrl Pts',(75.342557724821,3.60167218796151,-0.359366843973714));
#9669=CARTESIAN_POINT('Ctrl Pts',(75.342557724821,3.60728852407918,-0.32808146002479));
#9670=CARTESIAN_POINT('Ctrl Pts',(75.342557724821,3.61050399245623,-0.310169931824944));
#9671=CARTESIAN_POINT('Ctrl Pts',(75.342557724821,3.61359044725664,-0.292230814311455));
#9672=CARTESIAN_POINT('Ctrl Pts',(75.342557724821,3.61654486489718,-0.274281913907966));
#9673=CARTESIAN_POINT('Ctrl Pts',(75.342557724821,3.63581733262553,-0.157196367491248));
#9674=CARTESIAN_POINT('Ctrl Pts',(75.342557724821,3.64950486260566,-0.0395354677081342));
#9675=CARTESIAN_POINT('Ctrl Pts',(75.342557724821,3.65756797097238,0.0782629527285851));
#9676=CARTESIAN_POINT('Ctrl Pts',(75.342557724821,3.66562084842487,0.195911904067305));
#9677=CARTESIAN_POINT('Ctrl Pts',(75.342557724821,3.66806386102843,0.313698907639059));
#9678=CARTESIAN_POINT('Ctrl Pts',(75.342557724821,3.66481050835095,0.431210226129204));
#9679=CARTESIAN_POINT('Ctrl Pts',(75.342557724821,3.66155095575816,0.548945485979381));
#9680=CARTESIAN_POINT('Ctrl Pts',(75.342557724821,3.652573642136,0.666404895833316));
#9681=CARTESIAN_POINT('Ctrl Pts',(75.342557724821,3.6377394439107,0.783181642415076));
#9682=CARTESIAN_POINT('Ctrl Pts',(75.342557724821,3.63032234479805,0.841570015705956));
#9683=CARTESIAN_POINT('Ctrl Pts',(75.342557724821,3.62144017952809,0.899787785327359));
#9684=CARTESIAN_POINT('Ctrl Pts',(75.342557724821,3.61107027366315,0.957783896510187));
#9685=CARTESIAN_POINT('Ctrl Pts',(75.342557724821,3.60549862512678,0.988944637233916));
#9686=CARTESIAN_POINT('Ctrl Pts',(75.342557724821,3.59949743250429,1.02004138237487));
#9687=CARTESIAN_POINT('Ctrl Pts',(75.342557724821,3.59306273653391,1.05106613735378));
#9688=CARTESIAN_POINT('Ctrl Pts',(75.342557724821,3.58935704516694,1.06893305246783));
#9689=CARTESIAN_POINT('Ctrl Pts',(75.342557724821,3.5855075758258,1.08677609073766));
#9690=CARTESIAN_POINT('Ctrl Pts',(75.342557724821,3.58151352449986,1.10459371393155));
#9691=CARTESIAN_POINT('Ctrl Pts',(75.342557724821,3.57953485452689,1.11342064005904));
#9692=CARTESIAN_POINT('Ctrl Pts',(75.342557724821,3.57752094215402,1.12224021146939));
#9693=CARTESIAN_POINT('Ctrl Pts',(75.342557724821,3.57547241467767,1.13104933483286));
#9694=CARTESIAN_POINT('Ctrl Pts',(75.342557724821,3.54994667569026,1.24081568470107));
#9695=CARTESIAN_POINT('Ctrl Pts',(75.342557724821,3.51902110526928,1.34909263168916));
#9696=CARTESIAN_POINT('Ctrl Pts',(75.342557724821,3.4830615869259,1.45565358445287));
#9697=CARTESIAN_POINT('Ctrl Pts',(75.342557724821,3.4456917452281,1.56639383124708));
#9698=CARTESIAN_POINT('Ctrl Pts',(75.342557724821,3.40288528203317,1.67528140979421));
#9699=CARTESIAN_POINT('Ctrl Pts',(75.342557724821,3.35499628463391,1.78206193622134));
#9700=CARTESIAN_POINT('Ctrl Pts',(75.342557724821,3.30622973510779,1.89079918513508));
#9701=CARTESIAN_POINT('Ctrl Pts',(75.342557724821,3.25219236001142,1.99735212957777));
#9702=CARTESIAN_POINT('Ctrl Pts',(75.342557724821,3.19320376567024,2.10144246943319));
#9703=CARTESIAN_POINT('Ctrl Pts',(75.342557724821,3.15375302502262,2.17105662192186));
#9704=CARTESIAN_POINT('Ctrl Pts',(75.342557724821,3.11208660904809,2.23956910381198));
#9705=CARTESIAN_POINT('Ctrl Pts',(75.342557724821,3.06828808096117,2.30689197306326));
#9706=CARTESIAN_POINT('Ctrl Pts',(75.342557724821,3.04770324685026,2.33853299288607));
#9707=CARTESIAN_POINT('Ctrl Pts',(75.342557724821,3.02664732063322,2.36991117398798));
#9708=CARTESIAN_POINT('Ctrl Pts',(75.342557724821,3.00512831524903,2.40101699498357));
#9709=CARTESIAN_POINT('Ctrl Pts',(75.342557724821,2.99490091546237,2.41580074829069));
#9710=CARTESIAN_POINT('Ctrl Pts',(75.342557724821,2.98456791657202,2.43052436587747));
#9711=CARTESIAN_POINT('Ctrl Pts',(75.342557724821,2.9741332515261,2.4451824474385));
#9712=CARTESIAN_POINT('Ctrl Pts',(75.342557724821,2.90048108769345,2.54864522461958));
#9713=CARTESIAN_POINT('Ctrl Pts',(75.3425577248209,2.82202212090033,2.64849018376099));
#9714=CARTESIAN_POINT('Ctrl Pts',(75.3425577248209,2.7391739809035,2.74441746113153));
#9715=CARTESIAN_POINT('Ctrl Pts',(75.3425577248209,2.65815137026194,2.83823101499762));
#9716=CARTESIAN_POINT('Ctrl Pts',(75.3425577248209,2.57293010747928,2.92829830822171));
#9717=CARTESIAN_POINT('Ctrl Pts',(75.3425577248209,2.48384819044702,3.01432170978502));
#9718=CARTESIAN_POINT('Ctrl Pts',(75.3425577248209,2.39175560170328,3.10325241543698));
#9719=CARTESIAN_POINT('Ctrl Pts',(75.3425577248209,2.29553663680206,3.18786226001191));
#9720=CARTESIAN_POINT('Ctrl Pts',(75.3425577248209,2.19551580562984,3.26779099829018));
#9721=CARTESIAN_POINT('Ctrl Pts',(75.3425577248209,2.09549497445763,3.34771973656845));
#9722=CARTESIAN_POINT('Ctrl Pts',(75.3425577248209,1.99167161659826,3.42296825978045));
#9723=CARTESIAN_POINT('Ctrl Pts',(75.3425577248209,1.88433026752066,3.49313140215102));
#9724=CARTESIAN_POINT('Ctrl Pts',(77.0459088298365,-3.45658164681457,0.00280094662916092));
#9725=CARTESIAN_POINT('Ctrl Pts',(77.0364228182283,-3.45828790519784,0.196977771036481));
#9726=CARTESIAN_POINT('Ctrl Pts',(77.02693680662,-3.44332490726161,0.390891484629403));
#9727=CARTESIAN_POINT('Ctrl Pts',(77.0174507950117,-3.41075968470985,0.581802412792217));
#9728=CARTESIAN_POINT('Ctrl Pts',(76.9616210260054,-3.21909759027179,1.70540561509294));
#9729=CARTESIAN_POINT('Ctrl Pts',(76.905791256999,-2.41771342360892,2.72499556935934));
#9730=CARTESIAN_POINT('Ctrl Pts',(76.8499614879927,-1.37120627374349,3.17671705350414));
#9731=CARTESIAN_POINT('Ctrl Pts',(76.7941317189863,-0.324699123878052,3.62843853764894));
#9732=CARTESIAN_POINT('Ctrl Pts',(76.7383019499799,0.966931009189941,3.51229155167215));
#9733=CARTESIAN_POINT('Ctrl Pts',(76.6824721809736,1.91604094905346,2.88108016543812));
#9734=CARTESIAN_POINT('Ctrl Pts',(76.6266424119672,2.86515088891698,2.24986877920407));
#9735=CARTESIAN_POINT('Ctrl Pts',(76.5708126429609,3.47174063557601,1.10359299271277));
#9736=CARTESIAN_POINT('Ctrl Pts',(76.5149828739545,3.45983593312798,-0.0361595634637213));
#9737=CARTESIAN_POINT('Ctrl Pts',(76.4591531049482,3.44793123067995,-1.17591211964021));
#9738=CARTESIAN_POINT('Ctrl Pts',(76.4033233359418,2.81753207912487,-2.3091414455019));
#9739=CARTESIAN_POINT('Ctrl Pts',(76.3474935669354,1.85544410208129,-2.92042043852596));
#9740=CARTESIAN_POINT('Ctrl Pts',(76.291663797929,0.89335612503771,-3.53169943155002));
#9741=CARTESIAN_POINT('Ctrl Pts',(76.2358340289227,-0.400420677494361,-3.62102809173647));
#9742=CARTESIAN_POINT('Ctrl Pts',(76.1800042599164,-1.43726298495274,-3.14747114297997));
#9743=CARTESIAN_POINT('Ctrl Pts',(76.12417449091,-2.47410529241112,-2.67391419422347));
#9744=CARTESIAN_POINT('Ctrl Pts',(76.0683447219036,-3.25401310479582,-1.63747163652403));
#9745=CARTESIAN_POINT('Ctrl Pts',(76.0125149528973,-3.42216574953757,-0.510265666765961));
#9746=CARTESIAN_POINT('Ctrl Pts',(76.0042018007659,-3.44720397810103,-0.34242268842772));
#9747=CARTESIAN_POINT('Ctrl Pts',(75.9958886486346,-3.4586785296033,-0.172567327235602));
#9748=CARTESIAN_POINT('Ctrl Pts',(75.9875754965032,-3.45725565822888,-0.00252520199929829));
#9749=CARTESIAN_POINT('Origin',(75.342557724821,-5.12956166756098E-16,0.));
#9750=CARTESIAN_POINT('Ctrl Pts',(75.342557724821,-1.88729338390967,3.49128919534759));
#9751=CARTESIAN_POINT('Ctrl Pts',(75.342557724821,-1.98965881273553,3.42582705186126));
#9752=CARTESIAN_POINT('Ctrl Pts',(75.342557724821,-2.08853316026797,3.3554367053497));
#9753=CARTESIAN_POINT('Ctrl Pts',(75.342557724821,-2.18376353031218,3.28051395785925));
#9754=CARTESIAN_POINT('Ctrl Pts',(75.342557724821,-2.28075909933827,3.20420243536427));
#9755=CARTESIAN_POINT('Ctrl Pts',(75.342557724821,-2.37397483745187,3.12318822942394));
#9756=CARTESIAN_POINT('Ctrl Pts',(75.342557724821,-2.46321093678954,3.03785174096976));
#9757=CARTESIAN_POINT('Ctrl Pts',(75.342557724821,-2.55600352323115,2.94911418363274));
#9758=CARTESIAN_POINT('Ctrl Pts',(75.342557724821,-2.64449370202301,2.85570220672163));
#9759=CARTESIAN_POINT('Ctrl Pts',(75.342557724821,-2.72840589024478,2.75801402183562));
#9760=CARTESIAN_POINT('Ctrl Pts',(75.342557724821,-2.74149425994018,2.74277691378545));
#9761=CARTESIAN_POINT('Ctrl Pts',(75.342557724821,-2.75447114178973,2.72743572798769));
#9762=CARTESIAN_POINT('Ctrl Pts',(75.342557724821,-2.76733536476255,2.71199193333328));
#9763=CARTESIAN_POINT('Ctrl Pts',(75.342557724821,-2.78020766002005,2.69653844771603));
#9764=CARTESIAN_POINT('Ctrl Pts',(75.342557724821,-2.79296228879439,2.68098801714063));
#9765=CARTESIAN_POINT('Ctrl Pts',(75.342557724821,-2.80559444421283,2.66534725776366));
#9766=CARTESIAN_POINT('Ctrl Pts',(75.342557724821,-2.88250675556822,2.57011671988728));
#9767=CARTESIAN_POINT('Ctrl Pts',(75.342557724821,-2.95492997736749,2.47148290468358));
#9768=CARTESIAN_POINT('Ctrl Pts',(75.342557724821,-3.02267228602371,2.36982066191873));
#9769=CARTESIAN_POINT('Ctrl Pts',(75.342557724821,-3.09007944726784,2.26866138160448));
#9770=CARTESIAN_POINT('Ctrl Pts',(75.342557724821,-3.15285221813227,2.16450273906243));
#9771=CARTESIAN_POINT('Ctrl Pts',(75.342557724821,-3.21075473121433,2.05769343219054));
#9772=CARTESIAN_POINT('Ctrl Pts',(75.342557724821,-3.24743521561524,1.99003113385415));
#9773=CARTESIAN_POINT('Ctrl Pts',(75.342557724821,-3.28216028458533,1.92130473789008));
#9774=CARTESIAN_POINT('Ctrl Pts',(75.342557724821,-3.3148592707336,1.85160082777986));
#9775=CARTESIAN_POINT('Ctrl Pts',(75.342557724821,-3.33199284148589,1.81507746677503));
#9776=CARTESIAN_POINT('Ctrl Pts',(75.342557724821,-3.34857000106658,1.77828570999916));
#9777=CARTESIAN_POINT('Ctrl Pts',(75.342557724821,-3.36457961037642,1.74123797347753));
#9778=CARTESIAN_POINT('Ctrl Pts',(75.342557724821,-3.37260637694873,1.7226632832814));
#9779=CARTESIAN_POINT('Ctrl Pts',(75.342557724821,-3.38049087856411,1.70402302661623));
#9780=CARTESIAN_POINT('Ctrl Pts',(75.342557724821,-3.38822413051831,1.68533759572285));
#9781=CARTESIAN_POINT('Ctrl Pts',(75.342557724821,-3.43394894182751,1.57485525182781));
#9782=CARTESIAN_POINT('Ctrl Pts',(75.342557724821,-3.47445615533811,1.46264468374345));
#9783=CARTESIAN_POINT('Ctrl Pts',(75.342557724821,-3.50955062331665,1.3490487877896));
#9784=CARTESIAN_POINT('Ctrl Pts',(75.342557724821,-3.54398194376743,1.23759940785103));
#9785=CARTESIAN_POINT('Ctrl Pts',(75.342557724821,-3.57320329370337,1.12481579109674));
#9786=CARTESIAN_POINT('Ctrl Pts',(75.342557724821,-3.59698123988467,1.01101268319051));
#9787=CARTESIAN_POINT('Ctrl Pts',(75.342557724821,-3.62144613123762,0.893921802030013));
#9788=CARTESIAN_POINT('Ctrl Pts',(75.342557724821,-3.64014916389457,0.77575088847576));
#9789=CARTESIAN_POINT('Ctrl Pts',(75.342557724821,-3.65277727238172,0.656844752533057));
#9790=CARTESIAN_POINT('Ctrl Pts',(75.342557724821,-3.65909132662529,0.597391684561706));
#9791=CARTESIAN_POINT('Ctrl Pts',(75.342557724821,-3.66388568603325,0.537754916717839));
#9792=CARTESIAN_POINT('Ctrl Pts',(75.342557724821,-3.66711521089121,0.477978690984206));
#9793=CARTESIAN_POINT('Ctrl Pts',(75.342557724821,-3.6688033537149,0.446732358803051));
#9794=CARTESIAN_POINT('Ctrl Pts',(75.342557724821,-3.67006385615744,0.415447938173428));
#9795=CARTESIAN_POINT('Ctrl Pts',(75.342557724821,-3.67088981459646,0.384131877900408));
#9796=CARTESIAN_POINT('Ctrl Pts',(75.342557724821,-3.67138709308039,0.365277656865117));
#9797=CARTESIAN_POINT('Ctrl Pts',(75.342557724821,-3.67172685235443,0.346411968980907));
#9798=CARTESIAN_POINT('Ctrl Pts',(75.342557724821,-3.67190752969518,0.327536240136365));
#9799=CARTESIAN_POINT('Ctrl Pts',(75.342557724821,-3.6720008604043,0.317785791348867));
#9800=CARTESIAN_POINT('Ctrl Pts',(75.342557724821,-3.6720517296715,0.308032276855914));
#9801=CARTESIAN_POINT('Ctrl Pts',(75.342557724821,-3.67205995067616,0.298281359438954));
#9802=CARTESIAN_POINT('Ctrl Pts',(75.342557724821,-3.67215633969913,0.183954529334913));
#9803=CARTESIAN_POINT('Ctrl Pts',(75.342557724821,-3.66639691553994,0.0698132970449268));
#9804=CARTESIAN_POINT('Ctrl Pts',(75.342557724821,-3.65504660301135,-0.0437875909146339));
#9805=CARTESIAN_POINT('Ctrl Pts',(75.342557724821,-3.64352708680288,-0.15908197306051));
#9806=CARTESIAN_POINT('Ctrl Pts',(75.342557724821,-3.62624835841427,-0.273820618695414));
#9807=CARTESIAN_POINT('Ctrl Pts',(75.342557724821,-3.60343270120605,-0.38762384282797));
#9808=CARTESIAN_POINT('Ctrl Pts',(75.342557724821,-3.5805479808187,-0.501771550241523));
#9809=CARTESIAN_POINT('Ctrl Pts',(75.342557724821,-3.55209226834181,-0.614979001429506));
#9810=CARTESIAN_POINT('Ctrl Pts',(75.342557724821,-3.5182421068499,-0.726841589629112));
#9811=CARTESIAN_POINT('Ctrl Pts',(75.342557724821,-3.49759611478955,-0.795069155053657));
#9812=CARTESIAN_POINT('Ctrl Pts',(75.342557724821,-3.47494245755732,-0.862795951760317));
#9813=CARTESIAN_POINT('Ctrl Pts',(75.342557724821,-3.45031368885424,-0.92992425346773));
#9814=CARTESIAN_POINT('Ctrl Pts',(75.342557724821,-3.43733424954629,-0.965301081613749));
#9815=CARTESIAN_POINT('Ctrl Pts',(75.342557724821,-3.42380616879117,-1.00051160361389));
#9816=CARTESIAN_POINT('Ctrl Pts',(75.342557724821,-3.40973365029785,-1.03554089181167));
#9817=CARTESIAN_POINT('Ctrl Pts',(75.342557724821,-3.40339158387213,-1.05132755236583));
#9818=CARTESIAN_POINT('Ctrl Pts',(75.342557724821,-3.39693849996648,-1.06707827537105));
#9819=CARTESIAN_POINT('Ctrl Pts',(75.342557724821,-3.39038140719484,-1.08277623960184));
#9820=CARTESIAN_POINT('Ctrl Pts',(75.342557724821,-3.34615321126041,-1.18866045718896));
#9821=CARTESIAN_POINT('Ctrl Pts',(75.3425577248209,-3.29713139770849,-1.29231203608561));
#9822=CARTESIAN_POINT('Ctrl Pts',(75.3425577248209,-3.24352825182167,-1.39337011272125));
#9823=CARTESIAN_POINT('Ctrl Pts',(75.3425577248209,-3.19022134490429,-1.49386968966474));
#9824=CARTESIAN_POINT('Ctrl Pts',(75.3425577248209,-3.13238304795574,-1.59180509518516));
#9825=CARTESIAN_POINT('Ctrl Pts',(75.3425577248209,-3.07018008080428,-1.68679235709316));
#9826=CARTESIAN_POINT('Ctrl Pts',(75.3425577248209,-3.00962178257282,-1.7792681214857));
#9827=CARTESIAN_POINT('Ctrl Pts',(75.342557724821,-2.94492597991067,-1.86895010051926));
#9828=CARTESIAN_POINT('Ctrl Pts',(75.342557724821,-2.87621512332115,-1.95544730860172));
#9829=CARTESIAN_POINT('Ctrl Pts',(75.342557724821,-2.81023608483995,-2.03850554574002));
#9830=CARTESIAN_POINT('Ctrl Pts',(75.342557724821,-2.74055439650384,-2.11862751302659));
#9831=CARTESIAN_POINT('Ctrl Pts',(75.342557724821,-2.66725710276985,-2.19542711810058));
#9832=CARTESIAN_POINT('',(75.342557724821,-3.4544,-4.23041990297462E-16));
#9833=CARTESIAN_POINT('Origin',(75.342557724821,0.,0.));
#9834=CARTESIAN_POINT('Origin',(75.342557724821,0.,0.));
#9835=CARTESIAN_POINT('Ctrl Pts',(75.342557724821,-1.8872933839096,3.49128919534762));
#9836=CARTESIAN_POINT('Ctrl Pts',(75.3983874938273,-3.04449504617051,2.86573831175296));
#9837=CARTESIAN_POINT('Ctrl Pts',(75.5100470318401,-4.66829602391867,0.384128637822877));
#9838=CARTESIAN_POINT('Ctrl Pts',(75.6775363388591,-2.86406281752867,-3.71223393277672));
#9839=CARTESIAN_POINT('Ctrl Pts',(75.8450256458783,1.55028466462108,-4.42080615645044));
#9840=CARTESIAN_POINT('Ctrl Pts',(76.0125149528972,4.55194904417391,-1.11163115411373));
#9841=CARTESIAN_POINT('Ctrl Pts',(76.1800042599164,3.41272104871659,3.21148763121955));
#9842=CARTESIAN_POINT('Ctrl Pts',(76.3474935669354,-0.83234909652074,4.61115832194601));
#9843=CARTESIAN_POINT('Ctrl Pts',(76.5149828739545,-4.31977834004303,1.81565330639528));
#9844=CARTESIAN_POINT('Ctrl Pts',(76.6824721809736,-3.87667262829891,-2.63227689352042));
#9845=CARTESIAN_POINT('Ctrl Pts',(76.8499614879926,0.0939792462890116,-4.68487346091533));
#9846=CARTESIAN_POINT('Ctrl Pts',(77.0174507950118,3.9790823597631,-2.47467306941385));
#9847=CARTESIAN_POINT('Ctrl Pts',(77.1849401020308,4.24354045361218,1.98733341519075));
#9848=CARTESIAN_POINT('Ctrl Pts',(77.3524294090499,0.646690153391397,4.64099636386739));
#9849=CARTESIAN_POINT('Ctrl Pts',(77.519918716069,-3.53859451756145,3.07171589045833));
#9850=CARTESIAN_POINT('Ctrl Pts',(77.687408023088,-4.50402929941844,-1.29259812310088));
#9851=CARTESIAN_POINT('Ctrl Pts',(77.8548973301072,-1.3711384097138,-4.48074328527017));
#9852=CARTESIAN_POINT('Ctrl Pts',(78.0223866371261,3.00938367803536,-3.59175384599341));
#9853=CARTESIAN_POINT('Ctrl Pts',(78.1898759441454,4.65159553477052,0.565459445670238));
#9854=CARTESIAN_POINT('Ctrl Pts',(78.3573652511643,2.06120867216333,4.20814723864878));
#9855=CARTESIAN_POINT('Ctrl Pts',(78.5248545581835,-2.40472141992828,4.02174090914329));
#9856=CARTESIAN_POINT('Ctrl Pts',(78.6923438652025,-4.68253773972165,0.175855781190976));
#9857=CARTESIAN_POINT('Ctrl Pts',(78.8598331722217,-2.69960041692981,-3.83004470137668));
#9858=CARTESIAN_POINT('Ctrl Pts',(79.0273224792406,1.73976819338591,-4.35089548826393));
#9859=CARTESIAN_POINT('Ctrl Pts',(79.1948117862598,4.5960799186112,-0.912761895211113));
#9860=CARTESIAN_POINT('Ctrl Pts',(79.3623010932788,3.2703080678004,3.35591567615466));
#9861=CARTESIAN_POINT('Ctrl Pts',(79.529790400298,-1.03119568640402,4.57096492570699));
#9862=CARTESIAN_POINT('Ctrl Pts',(79.6972797073169,-4.39438970396336,1.62678333586707));
#9863=CARTESIAN_POINT('Ctrl Pts',(79.8647690143362,-3.75902292118467,-2.79764750621953));
#9864=CARTESIAN_POINT('Ctrl Pts',(80.032258321355,0.296769156290057,-4.67643164821721));
#9865=CARTESIAN_POINT('Ctrl Pts',(80.1997476283743,4.08252384642615,-2.30001824674852));
#9866=CARTESIAN_POINT('Ctrl Pts',(80.3672369353933,4.15349197522231,2.16923703262104));
#9867=CARTESIAN_POINT('Ctrl Pts',(80.5347262424123,0.445097936809096,4.66465140377808));
#9868=CARTESIAN_POINT('Ctrl Pts',(80.7022155494315,-3.66830141115372,2.91558735917221));
#9869=CARTESIAN_POINT('Ctrl Pts',(80.8697048564505,-4.44382514648826,-1.48643969251123));
#9870=CARTESIAN_POINT('Ctrl Pts',(81.0371941634697,-1.17580558461439,-4.53591954505886));
#9871=CARTESIAN_POINT('Ctrl Pts',(81.2046834704886,3.16210773630061,-3.45805719386958));
#9872=CARTESIAN_POINT('Ctrl Pts',(81.3721727775078,4.62274323446282,0.766374503930213));
#9873=CARTESIAN_POINT('Ctrl Pts',(81.5396620845268,1.87703356730924,4.29346362267612));
#9874=CARTESIAN_POINT('Ctrl Pts',(81.707151391546,-2.57663405263031,3.91382700829674));
#9875=CARTESIAN_POINT('Ctrl Pts',(81.874640698565,-4.68576042501116,-0.0270948601499234));
#9876=CARTESIAN_POINT('Ctrl Pts',(82.0421300055841,-2.53120077593259,-3.94336246418788));
#9877=CARTESIAN_POINT('Ctrl Pts',(82.2096193126032,1.92655929036014,-4.27146979303078));
#9878=CARTESIAN_POINT('Ctrl Pts',(82.3771086196222,4.63129675823398,-0.712864102910859));
#9879=CARTESIAN_POINT('Ctrl Pts',(82.5445979266413,3.12190600394933,3.49439376638532));
#9880=CARTESIAN_POINT('Ctrl Pts',(82.7120872336604,-1.22818205067104,4.52201876847685));
#9881=CARTESIAN_POINT('Ctrl Pts',(82.8795765406795,-4.46071774104712,1.43495021751798));
#9882=CARTESIAN_POINT('Ctrl Pts',(83.0470658476984,-3.63433915645072,-2.95781402186421));
#9883=CARTESIAN_POINT('Ctrl Pts',(83.2145551547178,0.499011969014512,-4.65919219895763));
#9884=CARTESIAN_POINT('Ctrl Pts',(83.3820444617366,4.17830011134652,-2.12105942197974));
#9885=CARTESIAN_POINT('Ctrl Pts',(83.5495337687558,4.05565256718464,2.34707629751062));
#9886=CARTESIAN_POINT('Ctrl Pts',(83.7170230757749,0.242669284494185,4.67955088768255));
#9887=CARTESIAN_POINT('Ctrl Pts',(83.8845123827939,-3.79112461211767,2.75398966364128));
#9888=CARTESIAN_POINT('Ctrl Pts',(84.0520016898132,-4.37528311379606,-1.6774929407239));
#9889=CARTESIAN_POINT('Ctrl Pts',(84.219490996832,-0.97826636104911,-4.58258440390215));
#9890=CARTESIAN_POINT('Ctrl Pts',(84.3869803038513,3.30889846384542,-3.31787218681023));
#9891=CARTESIAN_POINT('Ctrl Pts',(84.5544696108702,4.58521705524031,0.965851669968393));
#9892=CARTESIAN_POINT('Ctrl Pts',(84.7219589178894,1.68933645364314,4.37072388037037));
#9893=CARTESIAN_POINT('Ctrl Pts',(84.8894482249084,-2.74371198617596,3.79856939241103));
#9894=CARTESIAN_POINT('Ctrl Pts',(85.0569375319275,-4.68019095139554,-0.229994674987758));
#9895=CARTESIAN_POINT('Ctrl Pts',(85.2244268389466,-2.35805169304712,-4.04928106025811));
#9896=CARTESIAN_POINT('Ctrl Pts',(85.3919161459656,2.10973547078508,-4.18402929427589));
#9897=CARTESIAN_POINT('Ctrl Pts',(85.5594054529847,4.65782362744017,-0.511628720565475));
#9898=CARTESIAN_POINT('Ctrl Pts',(85.7268947600037,2.96764612613796,3.62631512172698));
#9899=CARTESIAN_POINT('Ctrl Pts',(85.894384067023,-1.42286390542218,4.46458768518373));
#9900=CARTESIAN_POINT('Ctrl Pts',(86.0618733740419,-4.5186758743998,1.24042461849348));
#9901=CARTESIAN_POINT('Ctrl Pts',(86.229362681061,-3.50283606998595,-3.11243061912276));
#9902=CARTESIAN_POINT('Ctrl Pts',(86.3968519880801,0.700318456568796,-4.63321043677455));
#9903=CARTESIAN_POINT('Ctrl Pts',(86.5643412950992,4.26623638905772,-1.93812073017321));
#9904=CARTESIAN_POINT('Ctrl Pts',(86.7318306021183,3.9502033026309,2.52051160678369));
#9905=CARTESIAN_POINT('Ctrl Pts',(86.8993199091373,0.0397852977070385,4.68566985842301));
#9906=CARTESIAN_POINT('Ctrl Pts',(87.0668092161565,-3.90683430574237,2.58722449731792));
#9907=CARTESIAN_POINT('Ctrl Pts',(87.2342985231754,-4.2985314832309,-1.86539861148232));
#9908=CARTESIAN_POINT('Ctrl Pts',(87.4017878301947,-0.778891559482246,-4.62065069342133));
#9909=CARTESIAN_POINT('Ctrl Pts',(87.5692771372135,3.44948051298471,-3.17146166342683));
#9910=CARTESIAN_POINT('Ctrl Pts',(87.7367664442328,4.53908736689592,1.16351655241039));
#9911=CARTESIAN_POINT('Ctrl Pts',(87.9042557512518,1.49846953985345,4.43978309494734));
#9912=CARTESIAN_POINT('Ctrl Pts',(88.071745058271,-2.90564173353642,3.67618430011031));
#9913=CARTESIAN_POINT('Ctrl Pts',(88.2392343652898,-4.66583976361946,-0.432462937455728));
#9914=CARTESIAN_POINT('Ctrl Pts',(88.4067236723092,-2.18047806078814,-4.1476017550482));
#9915=CARTESIAN_POINT('Ctrl Pts',(88.574212979328,2.28895303198969,-4.08873805829862));
#9916=CARTESIAN_POINT('Ctrl Pts',(88.7417022863472,4.67561075159403,-0.309433339534459));
#9917=CARTESIAN_POINT('Ctrl Pts',(88.9091915933663,2.80781788150847,3.75143221135632));
#9918=CARTESIAN_POINT('Ctrl Pts',(89.0766809003853,-1.614875957977,4.39877943664814));
#9919=CARTESIAN_POINT('Ctrl Pts',(89.2441702074045,-4.5681553537033,1.04357153872945));
#9920=CARTESIAN_POINT('Ctrl Pts',(89.4116595144236,-3.36476040873959,-3.26120718206482));
#9921=CARTESIAN_POINT('Ctrl Pts',(89.5791488214426,0.900310895961415,-4.59853511258327));
#9922=CARTESIAN_POINT('Ctrl Pts',(89.7466381284616,4.34616767952069,-1.75154543008276));
#9923=CARTESIAN_POINT('Ctrl Pts',(89.9141274354808,3.83734204230666,2.68921753416258));
#9924=CARTESIAN_POINT('Ctrl Pts',(90.0816167424998,-0.163173340857844,4.68299683371814));
#9925=CARTESIAN_POINT('Ctrl Pts',(90.2491060495189,-4.01521337859037,2.41560477313642));
#9926=CARTESIAN_POINT('Ctrl Pts',(90.416595356538,-4.21371426955079,-2.04980412993457));
#9927=CARTESIAN_POINT('Ctrl Pts',(90.584084663557,-0.578055276042246,-4.65004698078105));
#9928=CARTESIAN_POINT('Ctrl Pts',(90.7515739705762,3.58359009673503,-3.01910035578126));
#9929=CARTESIAN_POINT('Ctrl Pts',(90.9190632775952,4.48444073454358,1.35899828774903));
#9930=CARTESIAN_POINT('Ctrl Pts',(91.0865525846143,1.304790942286,4.5005116341675));
#9931=CARTESIAN_POINT('Ctrl Pts',(91.2540418916334,-3.06211942038283,3.54690147299146));
#9932=CARTESIAN_POINT('Ctrl Pts',(91.4215311986525,-4.64273386088492,-0.634119948295768));
#9933=CARTESIAN_POINT('Ctrl Pts',(91.5890205056715,-1.99881293045711,-4.2381396621777));
#9934=CARTESIAN_POINT('Ctrl Pts',(91.7565098126906,2.46387542085175,-3.98577567712814));
#9935=CARTESIAN_POINT('Ctrl Pts',(91.9239991197097,4.68462530132107,-0.10665579043167));
#9936=CARTESIAN_POINT('Ctrl Pts',(92.0914884267288,2.64272008949707,3.86950719504337));
#9937=CARTESIAN_POINT('Ctrl Pts',(92.2589777337479,-1.80385580473937,4.3247235657652));
#9938=CARTESIAN_POINT('Ctrl Pts',(92.4264670407669,-4.60906751720117,0.844748393393596));
#9939=CARTESIAN_POINT('Ctrl Pts',(92.593956347786,-3.22036301339166,-3.40384099298144));
#9940=CARTESIAN_POINT('Ctrl Pts',(92.761445654805,1.09859778933808,-4.55527773120639));
#9941=CARTESIAN_POINT('Ctrl Pts',(92.9289349618241,4.4179760167816,-1.56159205661129));
#9942=CARTESIAN_POINT('Ctrl Pts',(93.0964242688432,3.71721744660719,2.85269706473892));
#9943=CARTESIAN_POINT('Ctrl Pts',(93.2639135758623,-0.365701395163535,4.67189257704037));
#9944=CARTESIAN_POINT('Ctrl Pts',(93.4314028828815,-4.11630386768273,2.23875107871602));
#9945=CARTESIAN_POINT('Ctrl Pts',(93.5988921899004,-4.12050518287515,-2.22897883618675));
#9946=CARTESIAN_POINT('Ctrl Pts',(93.7663814969196,-0.377110979675515,-4.6734702206623));
#9947=CARTESIAN_POINT('Ctrl Pts',(93.9338708039386,3.71312449050035,-2.85538948225578));
#9948=CARTESIAN_POINT('Ctrl Pts',(94.0455303419513,4.18043603275127,0.073217031354101));
#9949=CARTESIAN_POINT('Ctrl Pts',(94.1013601109577,3.74476191969682,1.31443323424532));
#9950=CARTESIAN_POINT('Ctrl Pts',(75.2435710211684,-1.8057623097247,3.34046550210861));
#9951=CARTESIAN_POINT('Ctrl Pts',(75.2994007901748,-2.91297286017594,2.74193841668523));
#9952=CARTESIAN_POINT('Ctrl Pts',(75.4110603281875,-4.46662563568538,0.367534280668929));
#9953=CARTESIAN_POINT('Ctrl Pts',(75.5785496352065,-2.74033530381143,-3.55186542688076));
#9954=CARTESIAN_POINT('Ctrl Pts',(75.7460389422257,1.48331236710945,-4.22982733049178));
#9955=CARTESIAN_POINT('Ctrl Pts',(75.9135282492446,4.35530484546559,-1.06360868825602));
#9956=CARTESIAN_POINT('Ctrl Pts',(76.0810175562638,3.26529149941203,3.07275136555087));
#9957=CARTESIAN_POINT('Ctrl Pts',(76.2485068632828,-0.796391615551045,4.41195628243795));
#9958=CARTESIAN_POINT('Ctrl Pts',(76.415996170302,-4.13316391575316,1.73721708355901));
#9959=CARTESIAN_POINT('Ctrl Pts',(76.5834854773211,-3.7092003707564,-2.51856253172034));
#9960=CARTESIAN_POINT('Ctrl Pts',(76.7509747843401,0.0899193428493282,-4.48248692740379));
#9961=CARTESIAN_POINT('Ctrl Pts',(76.9184640913591,3.80718600182134,-2.36776719281517));
#9962=CARTESIAN_POINT('Ctrl Pts',(77.0859533983784,4.06021950601614,1.90148061165451));
#9963=CARTESIAN_POINT('Ctrl Pts',(77.2534427053972,0.618753138764886,4.44050532094832));
#9964=CARTESIAN_POINT('Ctrl Pts',(77.4209320124165,-3.38572723440279,2.93901776399053));
#9965=CARTESIAN_POINT('Ctrl Pts',(77.5884213194354,-4.30945523368357,-1.23675788418292));
#9966=CARTESIAN_POINT('Ctrl Pts',(77.7559106264547,-1.31190523041416,-4.28717517534649));
#9967=CARTESIAN_POINT('Ctrl Pts',(77.9233999334736,2.87937830314423,-3.4365900798465));
#9968=CARTESIAN_POINT('Ctrl Pts',(78.0908892404928,4.45064660766843,0.541031597617288));
#9969=CARTESIAN_POINT('Ctrl Pts',(78.2583785475117,1.97216445752588,4.02635527793915));
#9970=CARTESIAN_POINT('Ctrl Pts',(78.425867854531,-2.30083745458738,3.8480017018683));
#9971=CARTESIAN_POINT('Ctrl Pts',(78.5933571615498,-4.48025210936568,0.168258811443526));
#9972=CARTESIAN_POINT('Ctrl Pts',(78.7608464685692,-2.58297767891845,-3.66458677027721));
#9973=CARTESIAN_POINT('Ctrl Pts',(78.928335775588,1.66461020743164,-4.16293680317093));
#9974=CARTESIAN_POINT('Ctrl Pts',(79.0958250826073,4.3975292661272,-0.873330581337993));
#9975=CARTESIAN_POINT('Ctrl Pts',(79.2633143896262,3.12903075927143,3.21094011894477));
#9976=CARTESIAN_POINT('Ctrl Pts',(79.4308036966454,-0.986648032751362,4.37349924091645));
#9977=CARTESIAN_POINT('Ctrl Pts',(79.5982930036644,-4.20455206875214,1.55650629575761));
#9978=CARTESIAN_POINT('Ctrl Pts',(79.7657823106836,-3.59663313098949,-2.67678913395085));
#9979=CARTESIAN_POINT('Ctrl Pts',(79.9332716177025,0.283948728738327,-4.47440980101422));
#9980=CARTESIAN_POINT('Ctrl Pts',(80.1007609247218,3.90615881626054,-2.20065745848898));
#9981=CARTESIAN_POINT('Ctrl Pts',(80.2682502317407,3.9740611218927,2.07552599281181));
#9982=CARTESIAN_POINT('Ctrl Pts',(80.4357395387598,0.425869705938943,4.46313846313487));
#9983=CARTESIAN_POINT('Ctrl Pts',(80.6032288457789,-3.50983079019188,2.78963398525597));
#9984=CARTESIAN_POINT('Ctrl Pts',(80.770718152798,-4.25185190015997,-1.42222549779475));
#9985=CARTESIAN_POINT('Ctrl Pts',(80.9382074598171,-1.12501078335905,-4.33996782071231));
#9986=CARTESIAN_POINT('Ctrl Pts',(81.1056967668361,3.02550468209242,-3.30866912309442));
#9987=CARTESIAN_POINT('Ctrl Pts',(81.2731860738552,4.42304072673403,0.733267125360433));
#9988=CARTESIAN_POINT('Ctrl Pts',(81.4406753808743,1.79594571720148,4.10798599417651));
#9989=CARTESIAN_POINT('Ctrl Pts',(81.6081646878934,-2.46532346155667,3.74474968153832));
#9990=CARTESIAN_POINT('Ctrl Pts',(81.7756539949124,-4.48333557465068,-0.0259243621914455));
#9991=CARTESIAN_POINT('Ctrl Pts',(81.9431433019315,-2.4218529024123,-3.77300920573496));
#9992=CARTESIAN_POINT('Ctrl Pts',(82.1106326089505,1.84333192901658,-4.08694229797184));
#9993=CARTESIAN_POINT('Ctrl Pts',(82.2781219159698,4.43122473827827,-0.682068373665113));
#9994=CARTESIAN_POINT('Ctrl Pts',(82.4456112229886,2.98703966457872,3.34343595567747));
#9995=CARTESIAN_POINT('Ctrl Pts',(82.613100530008,-1.17512458608205,4.32666755767865));
#9996=CARTESIAN_POINT('Ctrl Pts',(82.7805898370269,-4.26801473463389,1.3729603681212));
#9997=CARTESIAN_POINT('Ctrl Pts',(82.948079144046,-3.47733570489205,-2.83003645611967));
#9998=CARTESIAN_POINT('Ctrl Pts',(83.1155684510651,0.477454651953081,-4.45791509596267));
#9999=CARTESIAN_POINT('Ctrl Pts',(83.2830577580841,3.99779754653636,-2.02942965495022));
#10000=CARTESIAN_POINT('Ctrl Pts',(83.4505470651032,3.88044837628226,2.24568260145816));
#10001=CARTESIAN_POINT('Ctrl Pts',(83.6180363721223,0.232185971404038,4.47739428933466));
#10002=CARTESIAN_POINT('Ctrl Pts',(83.7855256791413,-3.62734802887419,2.63501731017198));
#10003=CARTESIAN_POINT('Ctrl Pts',(83.9530149861606,-4.18627088328007,-1.60502524568462));
#10004=CARTESIAN_POINT('Ctrl Pts',(84.1205042931794,-0.936005254251792,
-4.38461675765357));
#10005=CARTESIAN_POINT('Ctrl Pts',(84.2879936001987,3.1659540502073,-3.17454010834003));
#10006=CARTESIAN_POINT('Ctrl Pts',(84.4554829072177,4.38713567845393,0.924126877825758));
#10007=CARTESIAN_POINT('Ctrl Pts',(84.6229722142368,1.61635711884576,4.18190860873838));
#10008=CARTESIAN_POINT('Ctrl Pts',(84.7904615212559,-2.62518362837316,3.63447119465887));
#10009=CARTESIAN_POINT('Ctrl Pts',(84.9579508282749,-4.47800670229525,-0.220058905028287));
#10010=CARTESIAN_POINT('Ctrl Pts',(85.125440135294,-2.25618385990748,-3.87435211845496));
#10011=CARTESIAN_POINT('Ctrl Pts',(85.2929294423131,2.01859489844716,-4.00327922876317));
#10012=CARTESIAN_POINT('Ctrl Pts',(85.4604187493321,4.45660564673476,-0.489526359837044));
#10013=CARTESIAN_POINT('Ctrl Pts',(85.6279080563512,2.83944381348879,3.46965830846837));
#10014=CARTESIAN_POINT('Ctrl Pts',(85.7953973633703,-1.36139618470794,4.2717174971838));
#10015=CARTESIAN_POINT('Ctrl Pts',(85.9628866703895,-4.32346907662573,1.18683827497456));
#10016=CARTESIAN_POINT('Ctrl Pts',(86.1303759774084,-3.35151355176255,-2.97797361637666));
#10017=CARTESIAN_POINT('Ctrl Pts',(86.2978652844277,0.67006469924502,-4.43305574590589));
#10018=CARTESIAN_POINT('Ctrl Pts',(86.4653545914465,4.08193497705043,-1.85439391462973));
#10019=CARTESIAN_POINT('Ctrl Pts',(86.6328438984658,3.77955451995724,2.41162550537063));
#10020=CARTESIAN_POINT('Ctrl Pts',(86.8003332054847,0.0380665728460967,
4.48324892053913));
#10021=CARTESIAN_POINT('Ctrl Pts',(86.9678225125039,-3.7380590637343,2.47545639903379));
#10022=CARTESIAN_POINT('Ctrl Pts',(87.135311819523,-4.11283492315532,-1.78481339146628));
#10023=CARTESIAN_POINT('Ctrl Pts',(87.3028011265419,-0.745243444112614,
-4.42103858346553));
#10024=CARTESIAN_POINT('Ctrl Pts',(87.4702904335612,3.30046295482377,-3.03445451956679));
#10025=CARTESIAN_POINT('Ctrl Pts',(87.63777974058,4.34299879264601,1.11325263734626));
#10026=CARTESIAN_POINT('Ctrl Pts',(87.8052690475994,1.43373565573179,4.24798446524562));
#10027=CARTESIAN_POINT('Ctrl Pts',(87.9727583546183,-2.78011801064765,3.51737313834554));
#10028=CARTESIAN_POINT('Ctrl Pts',(88.1402476616373,-4.46427548583109,-0.413780538557639));
#10029=CARTESIAN_POINT('Ctrl Pts',(88.3077369686566,-2.08628140856209,-3.96842535923012));
#10030=CARTESIAN_POINT('Ctrl Pts',(88.4752262756754,2.19007026100774,-3.91210457418012));
#10031=CARTESIAN_POINT('Ctrl Pts',(88.6427155826948,4.47362436712517,-0.296065819266569));
#10032=CARTESIAN_POINT('Ctrl Pts',(88.8102048897136,2.68652014902731,3.58937033982573));
#10033=CARTESIAN_POINT('Ctrl Pts',(88.9776941967329,-1.54511331659239,4.20875216498494));
#10034=CARTESIAN_POINT('Ctrl Pts',(89.1451835037518,-4.37081104242332,0.998489248256337));
#10035=CARTESIAN_POINT('Ctrl Pts',(89.3126728107711,-3.21940275908204,-3.12032303179962));
#10036=CARTESIAN_POINT('Ctrl Pts',(89.4801621177899,0.86141746525588,-4.39987839571967));
#10037=CARTESIAN_POINT('Ctrl Pts',(89.6476514248092,4.1584132357654,-1.67587866750318));
#10038=CARTESIAN_POINT('Ctrl Pts',(89.8151407318281,3.67156886607901,2.57304333668676));
#10039=CARTESIAN_POINT('Ctrl Pts',(89.9826300388473,-0.156124252532783,
4.48069137050152));
#10040=CARTESIAN_POINT('Ctrl Pts',(90.1501193458663,-3.84175616063527,2.31125064693693));
#10041=CARTESIAN_POINT('Ctrl Pts',(90.3176086528854,-4.0316818131062,-1.9612525915214));
#10042=CARTESIAN_POINT('Ctrl Pts',(90.4850979599046,-0.553083288117217,
-4.4491649512113));
#10043=CARTESIAN_POINT('Ctrl Pts',(90.6525872669235,3.42877900455607,-2.88867522041151));
#10044=CARTESIAN_POINT('Ctrl Pts',(90.8200765739428,4.2907128948113,1.30028956171827));
#10045=CARTESIAN_POINT('Ctrl Pts',(90.9875658809616,1.24842397357924,4.30608953157147));
#10046=CARTESIAN_POINT('Ctrl Pts',(91.1550551879809,-2.92983586142229,3.39367532935823));
#10047=CARTESIAN_POINT('Ctrl Pts',(91.3225444949997,-4.4421677580947,-0.606725966529394));
#10048=CARTESIAN_POINT('Ctrl Pts',(91.4900338020191,-1.91246421186136,-4.05505202877162));
#10049=CARTESIAN_POINT('Ctrl Pts',(91.657523109038,2.35743600267096,-3.81359016787621));
#10050=CARTESIAN_POINT('Ctrl Pts',(91.825012416057,4.482249488304,-0.102048260285022));
#10051=CARTESIAN_POINT('Ctrl Pts',(91.9925017230764,2.5285545816308,3.7023444842175));
#10052=CARTESIAN_POINT('Ctrl Pts',(92.1599910300952,-1.72592923397463,4.13789550772414));
#10053=CARTESIAN_POINT('Ctrl Pts',(92.3274803371144,-4.40995580045808,0.808255262798993));
#10054=CARTESIAN_POINT('Ctrl Pts',(92.4949696441334,-3.08124333121314,-3.25679506208464));
#10055=CARTESIAN_POINT('Ctrl Pts',(92.6624589511525,1.05113836483867,-4.35848973321828));
#10056=CARTESIAN_POINT('Ctrl Pts',(92.8299482581715,4.22711945285663,-1.49413127976568));
#10057=CARTESIAN_POINT('Ctrl Pts',(92.9974375651909,3.55663365291376,2.7294605515422));
#10058=CARTESIAN_POINT('Ctrl Pts',(93.1649268722096,-0.349903094892468,
4.47006681771222));
#10059=CARTESIAN_POINT('Ctrl Pts',(93.3324161792289,-3.93847954059884,2.14203703211549));
#10060=CARTESIAN_POINT('Ctrl Pts',(93.4999054862479,-3.94249935897495,-2.13268695046349));
#10061=CARTESIAN_POINT('Ctrl Pts',(93.667394793267,-0.360819785353534,-4.47157630712969));
#10062=CARTESIAN_POINT('Ctrl Pts',(93.834884100286,3.55271751251074,-2.73203665662233));
#10063=CARTESIAN_POINT('Ctrl Pts',(93.9465436382988,3.99984119613641,0.0700540555996051));
#10064=CARTESIAN_POINT('Ctrl Pts',(94.0023734073051,3.58298820476592,1.25764971852592));
#10065=CARTESIAN_POINT('Ctrl Pts',(75.1445843175159,-1.72423123553981,3.18964180886959));
#10066=CARTESIAN_POINT('Ctrl Pts',(75.2004140865222,-2.78145067418138,2.6181385216175));
#10067=CARTESIAN_POINT('Ctrl Pts',(75.312073624535,-4.26495524745209,0.35093992351498));
#10068=CARTESIAN_POINT('Ctrl Pts',(75.4795629315539,-2.6166077900942,-3.39149692098481));
#10069=CARTESIAN_POINT('Ctrl Pts',(75.6470522385733,1.41634006959782,-4.03884850453312));
#10070=CARTESIAN_POINT('Ctrl Pts',(75.814541545592,4.15866064675728,-1.0155862223983));
#10071=CARTESIAN_POINT('Ctrl Pts',(75.9820308526114,3.11786195010748,2.93401509988218));
#10072=CARTESIAN_POINT('Ctrl Pts',(76.1495201596302,-0.760434134581352,
4.21275424292987));
#10073=CARTESIAN_POINT('Ctrl Pts',(76.3170094666494,-3.9465494914633,1.65878086072273));
#10074=CARTESIAN_POINT('Ctrl Pts',(76.4844987736685,-3.54172811321389,-2.40484816992026));
#10075=CARTESIAN_POINT('Ctrl Pts',(76.6519880806875,0.0858594394096438,
-4.28010039389224));
#10076=CARTESIAN_POINT('Ctrl Pts',(76.8194773877067,3.63528964387957,-2.26086131621649));
#10077=CARTESIAN_POINT('Ctrl Pts',(76.9869666947257,3.87689855842009,1.81562780811827));
#10078=CARTESIAN_POINT('Ctrl Pts',(77.1544560017448,0.590816124138375,4.24001427802925));
#10079=CARTESIAN_POINT('Ctrl Pts',(77.3219453087639,-3.23285995124413,2.80631963752273));
#10080=CARTESIAN_POINT('Ctrl Pts',(77.4894346157829,-4.1148811679487,-1.18091764526496));
#10081=CARTESIAN_POINT('Ctrl Pts',(77.6569239228021,-1.25267205111452,-4.09360706542282));
#10082=CARTESIAN_POINT('Ctrl Pts',(77.8244132298211,2.7493729282531,-3.28142631369958));
#10083=CARTESIAN_POINT('Ctrl Pts',(77.9919025368402,4.24969768056634,0.516603749564329));
#10084=CARTESIAN_POINT('Ctrl Pts',(78.1593918438592,1.88312024288842,3.84456331722953));
#10085=CARTESIAN_POINT('Ctrl Pts',(78.3268811508785,-2.19695348924648,3.67426249459331));
#10086=CARTESIAN_POINT('Ctrl Pts',(78.4943704578973,-4.2779664790097,0.160661841696076));
#10087=CARTESIAN_POINT('Ctrl Pts',(78.6618597649166,-2.46635494090708,-3.49912883917774));
#10088=CARTESIAN_POINT('Ctrl Pts',(78.8293490719354,1.58945222147737,-3.97497811807793));
#10089=CARTESIAN_POINT('Ctrl Pts',(78.9968383789548,4.19897861364319,-0.833899267464873));
#10090=CARTESIAN_POINT('Ctrl Pts',(79.1643276859736,2.98775345074245,3.06596456173489));
#10091=CARTESIAN_POINT('Ctrl Pts',(79.3318169929929,-0.94210037909871,4.17603355612591));
#10092=CARTESIAN_POINT('Ctrl Pts',(79.4993063000118,-4.01471443354093,1.48622925564816));
#10093=CARTESIAN_POINT('Ctrl Pts',(79.6667956070311,-3.43424334079431,-2.55593076168216));
#10094=CARTESIAN_POINT('Ctrl Pts',(79.8342849140499,0.271128301186596,-4.27238795381124));
#10095=CARTESIAN_POINT('Ctrl Pts',(80.0017742210692,3.72979378609493,-2.10129667022944));
#10096=CARTESIAN_POINT('Ctrl Pts',(80.1692635280881,3.7946302685631,1.98181495300258));
#10097=CARTESIAN_POINT('Ctrl Pts',(80.3367528351073,0.406641475068789,4.26162552249166));
#10098=CARTESIAN_POINT('Ctrl Pts',(80.5042421421263,-3.35136016923003,2.66368061133973));
#10099=CARTESIAN_POINT('Ctrl Pts',(80.6717314491454,-4.05987865383168,-1.35801130307826));
#10100=CARTESIAN_POINT('Ctrl Pts',(80.8392207561645,-1.07421598210371,-4.14401609636577));
#10101=CARTESIAN_POINT('Ctrl Pts',(81.0067100631835,2.88890162788424,-3.15928105231925));
#10102=CARTESIAN_POINT('Ctrl Pts',(81.1741993702027,4.22333821900523,0.700159746790646));
#10103=CARTESIAN_POINT('Ctrl Pts',(81.3416886772216,1.71485786709373,3.9225083656769));
#10104=CARTESIAN_POINT('Ctrl Pts',(81.5091779842409,-2.35401287048305,3.5756723547799));
#10105=CARTESIAN_POINT('Ctrl Pts',(81.6766672912598,-4.28091072429019,-0.0247538642329713));
#10106=CARTESIAN_POINT('Ctrl Pts',(81.844156598279,-2.31250502889201,-3.60265594728204));
#10107=CARTESIAN_POINT('Ctrl Pts',(82.0116459052979,1.76010456767303,-3.90241480291292));
#10108=CARTESIAN_POINT('Ctrl Pts',(82.1791352123172,4.23115271832256,-0.651272644419364));
#10109=CARTESIAN_POINT('Ctrl Pts',(82.3466245193362,2.85217332520811,3.19247814496963));
#10110=CARTESIAN_POINT('Ctrl Pts',(82.5141138263553,-1.12206712149307,4.13131634688045));
#10111=CARTESIAN_POINT('Ctrl Pts',(82.6816031333744,-4.07531172822065,1.31097051872443));
#10112=CARTESIAN_POINT('Ctrl Pts',(82.8490924403933,-3.32033225333338,-2.70225889037514));
#10113=CARTESIAN_POINT('Ctrl Pts',(83.0165817474127,0.455897334891659,-4.2566379929677));
#10114=CARTESIAN_POINT('Ctrl Pts',(83.1840710544314,3.81729498172618,-1.93779988792069));
#10115=CARTESIAN_POINT('Ctrl Pts',(83.3515603614509,3.70524418537989,2.1442889054057));
#10116=CARTESIAN_POINT('Ctrl Pts',(83.5190496684696,0.221702658313887,4.27523769098678));
#10117=CARTESIAN_POINT('Ctrl Pts',(83.6865389754889,-3.4635714456307,2.51604495670267));
#10118=CARTESIAN_POINT('Ctrl Pts',(83.8540282825079,-3.99725865276408,-1.53255755064535));
#10119=CARTESIAN_POINT('Ctrl Pts',(84.0215175895269,-0.893744147454468,
-4.186649111405));
#10120=CARTESIAN_POINT('Ctrl Pts',(84.1890068965461,3.02300963656918,-3.03120802986982));
#10121=CARTESIAN_POINT('Ctrl Pts',(84.3564962035651,4.18905430166755,0.882402085683122));
#10122=CARTESIAN_POINT('Ctrl Pts',(84.5239855105842,1.54337778404837,3.99309333710638));
#10123=CARTESIAN_POINT('Ctrl Pts',(84.6914748176033,-2.50665527057035,3.47037299690671));
#10124=CARTESIAN_POINT('Ctrl Pts',(84.8589641246224,-4.27582245319496,-0.210123135068815));
#10125=CARTESIAN_POINT('Ctrl Pts',(85.0264534316414,-2.15431602676784,-3.69942317665181));
#10126=CARTESIAN_POINT('Ctrl Pts',(85.1939427386606,1.92745432610924,-3.82252916325045));
#10127=CARTESIAN_POINT('Ctrl Pts',(85.3614320456795,4.25538766602934,-0.467423999108614));
#10128=CARTESIAN_POINT('Ctrl Pts',(85.5289213526986,2.71124150083964,3.31300149520976));
#10129=CARTESIAN_POINT('Ctrl Pts',(85.6964106597178,-1.2999284639937,4.07884730918386));
#10130=CARTESIAN_POINT('Ctrl Pts',(85.8638999667367,-4.12826227885166,1.13325193145564));
#10131=CARTESIAN_POINT('Ctrl Pts',(86.031389273756,-3.20019103353916,-2.84351661363055));
#10132=CARTESIAN_POINT('Ctrl Pts',(86.1988785807749,0.63981094192125,-4.23290105503723));
#10133=CARTESIAN_POINT('Ctrl Pts',(86.3663678877942,3.89763356504313,-1.77066709908625));
#10134=CARTESIAN_POINT('Ctrl Pts',(86.5338571948131,3.60890573728359,2.30273940395758));
#10135=CARTESIAN_POINT('Ctrl Pts',(86.7013465018323,0.0363478479851531,
4.28082798265526));
#10136=CARTESIAN_POINT('Ctrl Pts',(86.8688358088512,-3.56928382172623,2.36368830074965));
#10137=CARTESIAN_POINT('Ctrl Pts',(87.0363251158705,-3.92713836307975,-1.70422817145024));
#10138=CARTESIAN_POINT('Ctrl Pts',(87.2038144228895,-0.71159532874298,-4.22142647350973));
#10139=CARTESIAN_POINT('Ctrl Pts',(87.3713037299085,3.15144539666283,-2.89744737570675));
#10140=CARTESIAN_POINT('Ctrl Pts',(87.5387930369278,4.14691021839611,1.06298872228213));
#10141=CARTESIAN_POINT('Ctrl Pts',(87.7062823439466,1.36900177161012,4.05618583554389));
#10142=CARTESIAN_POINT('Ctrl Pts',(87.8737716509658,-2.65459428775888,3.35856197658078));
#10143=CARTESIAN_POINT('Ctrl Pts',(88.0412609579848,-4.26271120804273,-0.39509813965955));
#10144=CARTESIAN_POINT('Ctrl Pts',(88.208750265004,-1.99208475633604,-3.78924896341204));
#10145=CARTESIAN_POINT('Ctrl Pts',(88.3762395720229,2.09118749002578,-3.73547109006162));
#10146=CARTESIAN_POINT('Ctrl Pts',(88.5437288790422,4.2716379826563,-0.282698298998683));
#10147=CARTESIAN_POINT('Ctrl Pts',(88.7112181860611,2.56522241654614,3.42730846829514));
#10148=CARTESIAN_POINT('Ctrl Pts',(88.8787074930802,-1.47535067520778,4.01872489332174));
#10149=CARTESIAN_POINT('Ctrl Pts',(89.0461968000995,-4.17346673114334,0.953406957783226));
#10150=CARTESIAN_POINT('Ctrl Pts',(89.2136861071183,-3.07404510942449,-2.97943888153443));
#10151=CARTESIAN_POINT('Ctrl Pts',(89.3811754141374,0.822524034550345,-4.20122167885608));
#10152=CARTESIAN_POINT('Ctrl Pts',(89.5486647211566,3.97065879201011,-1.60021190492361));
#10153=CARTESIAN_POINT('Ctrl Pts',(89.7161540281756,3.50579568985136,2.45686913921093));
#10154=CARTESIAN_POINT('Ctrl Pts',(89.8836433351946,-0.149075164207724,
4.2783859072849));
#10155=CARTESIAN_POINT('Ctrl Pts',(90.0511326422139,-3.66829894268017,2.20689652073743));
#10156=CARTESIAN_POINT('Ctrl Pts',(90.2186219492327,-3.8496493566616,-1.87270105310823));
#10157=CARTESIAN_POINT('Ctrl Pts',(90.3861112562521,-0.528111300192195,
-4.24828292164156));
#10158=CARTESIAN_POINT('Ctrl Pts',(90.5536005632709,3.27396791237712,-2.75825008504176));
#10159=CARTESIAN_POINT('Ctrl Pts',(90.7210898702902,4.09698505507901,1.24158083568751));
#10160=CARTESIAN_POINT('Ctrl Pts',(90.888579177309,1.19205700487249,4.11166742897543));
#10161=CARTESIAN_POINT('Ctrl Pts',(91.0560684843284,-2.79755230246175,3.240449185725));
#10162=CARTESIAN_POINT('Ctrl Pts',(91.2235577913473,-4.24160165530447,-0.579331984763014));
#10163=CARTESIAN_POINT('Ctrl Pts',(91.3910470983663,-1.82611549326562,-3.87196439536554));
#10164=CARTESIAN_POINT('Ctrl Pts',(91.5585364053856,2.25099658449016,-3.64140465862427));
#10165=CARTESIAN_POINT('Ctrl Pts',(91.7260257124045,4.27987367528693,-0.0974407301383736));
#10166=CARTESIAN_POINT('Ctrl Pts',(91.8935150194238,2.41438907376452,3.53518177339162));
#10167=CARTESIAN_POINT('Ctrl Pts',(92.0610043264426,-1.64800266320989,3.95106744968309));
#10168=CARTESIAN_POINT('Ctrl Pts',(92.2284936334618,-4.21084408371499,0.771762132204391));
#10169=CARTESIAN_POINT('Ctrl Pts',(92.3959829404809,-2.94212364903462,-3.10974913118785));
#10170=CARTESIAN_POINT('Ctrl Pts',(92.5634722474998,1.00367894033927,-4.16170173523016));
#10171=CARTESIAN_POINT('Ctrl Pts',(92.7309615545192,4.03626288893166,-1.42667050292008));
#10172=CARTESIAN_POINT('Ctrl Pts',(92.8984508615381,3.39604985922033,2.60622403834548));
#10173=CARTESIAN_POINT('Ctrl Pts',(93.0659401685572,-0.334104794621406,
4.26824105838408));
#10174=CARTESIAN_POINT('Ctrl Pts',(93.2334294755763,-3.76065521351494,2.04532298551495));
#10175=CARTESIAN_POINT('Ctrl Pts',(93.4009187825955,-3.76449353507474,-2.03639506474021));
#10176=CARTESIAN_POINT('Ctrl Pts',(93.5684080896143,-0.344528591031553,
-4.26968239359708));
#10177=CARTESIAN_POINT('Ctrl Pts',(93.7358973966336,3.39231053452112,-2.60868383098888));
#10178=CARTESIAN_POINT('Ctrl Pts',(93.8475569346462,3.81924635952156,0.0668910798451053));
#10179=CARTESIAN_POINT('Ctrl Pts',(93.9033867036526,3.42121448983501,1.20086620280652));
#10180=CARTESIAN_POINT('Ctrl Pts',(75.0455976138633,-1.64270016135492,3.03881811563057));
#10181=CARTESIAN_POINT('Ctrl Pts',(75.1014273828696,-2.64992848818681,2.49433862654978));
#10182=CARTESIAN_POINT('Ctrl Pts',(75.2130869208824,-4.06328485921881,0.334345566361032));
#10183=CARTESIAN_POINT('Ctrl Pts',(75.3805762279014,-2.49288027637696,-3.23112841508885));
#10184=CARTESIAN_POINT('Ctrl Pts',(75.5480655349206,1.34936777208619,-3.84786967857446));
#10185=CARTESIAN_POINT('Ctrl Pts',(75.7155548419395,3.96201644804897,-0.96756375654059));
#10186=CARTESIAN_POINT('Ctrl Pts',(75.8830441489588,2.97043240080292,2.7952788342135));
#10187=CARTESIAN_POINT('Ctrl Pts',(76.0505334559776,-0.724476653611653,
4.01355220342181));
#10188=CARTESIAN_POINT('Ctrl Pts',(76.2180227629969,-3.75993506717345,1.58034463788646));
#10189=CARTESIAN_POINT('Ctrl Pts',(76.3855120700159,-3.37425585567137,-2.29113380812018));
#10190=CARTESIAN_POINT('Ctrl Pts',(76.553001377035,0.0817995359699572,-4.0777138603807));
#10191=CARTESIAN_POINT('Ctrl Pts',(76.7204906840541,3.4633932859378,-2.15395543961782));
#10192=CARTESIAN_POINT('Ctrl Pts',(76.8879799910732,3.69357761082405,1.72977500458203));
#10193=CARTESIAN_POINT('Ctrl Pts',(77.0554692980922,0.562879109511871,4.03952323511018));
#10194=CARTESIAN_POINT('Ctrl Pts',(77.2229586051114,-3.07999266808548,2.67362151105493));
#10195=CARTESIAN_POINT('Ctrl Pts',(77.3904479121303,-3.92030710221381,-1.12507740634701));
#10196=CARTESIAN_POINT('Ctrl Pts',(77.5579372191495,-1.19343887181489,-3.90003895549915));
#10197=CARTESIAN_POINT('Ctrl Pts',(77.7254265261685,2.61936755336198,-3.12626254755267));
#10198=CARTESIAN_POINT('Ctrl Pts',(77.8929158331876,4.04874875346425,0.492175901511377));
#10199=CARTESIAN_POINT('Ctrl Pts',(78.0604051402066,1.79407602825097,3.6627713565199));
#10200=CARTESIAN_POINT('Ctrl Pts',(78.2278944472258,-2.09306952390558,3.50052328731832));
#10201=CARTESIAN_POINT('Ctrl Pts',(78.3953837542448,-4.07568084865373,0.153064871948625));
#10202=CARTESIAN_POINT('Ctrl Pts',(78.562873061264,-2.34973220289571,-3.33367090807826));
#10203=CARTESIAN_POINT('Ctrl Pts',(78.730362368283,1.5142942355231,-3.78701943298493));
#10204=CARTESIAN_POINT('Ctrl Pts',(78.8978516753021,4.00042796115919,-0.794467953591753));
#10205=CARTESIAN_POINT('Ctrl Pts',(79.0653409823211,2.84647614221347,2.92098900452501));
#10206=CARTESIAN_POINT('Ctrl Pts',(79.2328302893403,-0.897552725446056,
3.97856787133537));
#10207=CARTESIAN_POINT('Ctrl Pts',(79.4003195963593,-3.82487679832971,1.4159522155387));
#10208=CARTESIAN_POINT('Ctrl Pts',(79.5678089033784,-3.27185355059914,-2.43507238941348));
#10209=CARTESIAN_POINT('Ctrl Pts',(79.7352982103974,0.258307873634867,-4.07036610660826));
#10210=CARTESIAN_POINT('Ctrl Pts',(79.9027875174166,3.55342875592932,-2.00193588196991));
#10211=CARTESIAN_POINT('Ctrl Pts',(80.0702768244356,3.6151994152335,1.88810391319336));
#10212=CARTESIAN_POINT('Ctrl Pts',(80.2377661314546,0.387413244198636,4.06011258184844));
#10213=CARTESIAN_POINT('Ctrl Pts',(80.4052554384739,-3.19288954826819,2.53772723742349));
#10214=CARTESIAN_POINT('Ctrl Pts',(80.5727447454928,-3.86790540750339,-1.29379710836178));
#10215=CARTESIAN_POINT('Ctrl Pts',(80.740234052512,-1.02342118084837,-3.94806437201922));
#10216=CARTESIAN_POINT('Ctrl Pts',(80.907723359531,2.75229857367605,-3.00989298154409));
#10217=CARTESIAN_POINT('Ctrl Pts',(81.0752126665501,4.02363571127644,0.667052368220863));
#10218=CARTESIAN_POINT('Ctrl Pts',(81.2427019735692,1.63377001698596,3.73703073717729));
#10219=CARTESIAN_POINT('Ctrl Pts',(81.4101912805883,-2.24270227940942,3.40659502802148));
#10220=CARTESIAN_POINT('Ctrl Pts',(81.5776805876073,-4.07848587392971,-0.0235833662744953));
#10221=CARTESIAN_POINT('Ctrl Pts',(81.7451698946264,-2.20315715537172,-3.43230268882913));
#10222=CARTESIAN_POINT('Ctrl Pts',(81.9126592016455,1.67687720632947,-3.71788730785399));
#10223=CARTESIAN_POINT('Ctrl Pts',(82.0801485086645,4.03108069836686,-0.620476915173612));
#10224=CARTESIAN_POINT('Ctrl Pts',(82.2476378156836,2.7173069858375,3.04152033426178));
#10225=CARTESIAN_POINT('Ctrl Pts',(82.4151271227027,-1.06900965690408,3.93596513608225));
#10226=CARTESIAN_POINT('Ctrl Pts',(82.5826164297217,-3.88260872180742,1.24898066932765));
#10227=CARTESIAN_POINT('Ctrl Pts',(82.7501057367409,-3.1633288017747,-2.5744813246306));
#10228=CARTESIAN_POINT('Ctrl Pts',(82.9175950437599,0.434340017830227,-4.05536088997273));
#10229=CARTESIAN_POINT('Ctrl Pts',(83.0850843507791,3.63679241691602,-1.84617012089117));
#10230=CARTESIAN_POINT('Ctrl Pts',(83.252573657798,3.53003999447751,2.04289520935324));
#10231=CARTESIAN_POINT('Ctrl Pts',(83.4200629648173,0.21121934522374,4.07308109263889));
#10232=CARTESIAN_POINT('Ctrl Pts',(83.5875522718362,-3.29979486238722,2.39707260323337));
#10233=CARTESIAN_POINT('Ctrl Pts',(83.7550415788554,-3.80824642224809,-1.46008985560608));
#10234=CARTESIAN_POINT('Ctrl Pts',(83.9225308858744,-0.851483040657149,
-3.98868146515643));
#10235=CARTESIAN_POINT('Ctrl Pts',(84.0900201928935,2.88006522293106,-2.88787595139962));
#10236=CARTESIAN_POINT('Ctrl Pts',(84.2575094999126,3.99097292488117,0.840677293540489));
#10237=CARTESIAN_POINT('Ctrl Pts',(84.4249988069316,1.47039844925099,3.80427806547437));
#10238=CARTESIAN_POINT('Ctrl Pts',(84.5924881139508,-2.38812691276755,3.30627479915456));
#10239=CARTESIAN_POINT('Ctrl Pts',(84.7599774209698,-4.07363820409468,-0.200187365109346));
#10240=CARTESIAN_POINT('Ctrl Pts',(84.9274667279889,-2.05244819362821,-3.52449423484866));
#10241=CARTESIAN_POINT('Ctrl Pts',(85.094956035008,1.83631375377133,-3.64177909773774));
#10242=CARTESIAN_POINT('Ctrl Pts',(85.262445342027,4.05416968532392,-0.445321638380185));
#10243=CARTESIAN_POINT('Ctrl Pts',(85.4299346490461,2.58303918819047,3.15634468195116));
#10244=CARTESIAN_POINT('Ctrl Pts',(85.5974239560652,-1.23846074327946,3.88597712118393));
#10245=CARTESIAN_POINT('Ctrl Pts',(85.7649132630843,-3.93305548107759,1.07966558793672));
#10246=CARTESIAN_POINT('Ctrl Pts',(85.9324025701033,-3.04886851531577,-2.70905961088445));
#10247=CARTESIAN_POINT('Ctrl Pts',(86.0998918771225,0.609557184597477,-4.03274636416857));
#10248=CARTESIAN_POINT('Ctrl Pts',(86.2673811841414,3.71333215303584,-1.68694028354276));
#10249=CARTESIAN_POINT('Ctrl Pts',(86.4348704911607,3.43825695460993,2.19385330254452));
#10250=CARTESIAN_POINT('Ctrl Pts',(86.6023597981796,0.0346291231242072,
4.07840704477139));
#10251=CARTESIAN_POINT('Ctrl Pts',(86.7698491051988,-3.40050857971816,2.25192020246552));
#10252=CARTESIAN_POINT('Ctrl Pts',(86.9373384122178,-3.74144180300417,-1.62364295143421));
#10253=CARTESIAN_POINT('Ctrl Pts',(87.104827719237,-0.677947213373348,-4.02181436355392));
#10254=CARTESIAN_POINT('Ctrl Pts',(87.2723170262559,3.00242783850189,-2.76044023184671));
#10255=CARTESIAN_POINT('Ctrl Pts',(87.4398063332751,3.9508216441462,1.012724807218));
#10256=CARTESIAN_POINT('Ctrl Pts',(87.6072956402942,1.30426788748845,3.86438720584216));
#10257=CARTESIAN_POINT('Ctrl Pts',(87.7747849473132,-2.52907056487011,3.19975081481601));
#10258=CARTESIAN_POINT('Ctrl Pts',(87.9422742543322,-4.06114693025437,-0.376415740761465));
#10259=CARTESIAN_POINT('Ctrl Pts',(88.1097635613515,-1.89788810411,-3.61007256759395));
#10260=CARTESIAN_POINT('Ctrl Pts',(88.2772528683704,1.99230471904383,-3.55883760594312));
#10261=CARTESIAN_POINT('Ctrl Pts',(88.4447421753896,4.06965159818744,-0.269330778730792));
#10262=CARTESIAN_POINT('Ctrl Pts',(88.6122314824086,2.44392468406498,3.26524659676454));
#10263=CARTESIAN_POINT('Ctrl Pts',(88.7797207894276,-1.40558803382318,3.82869762165855));
#10264=CARTESIAN_POINT('Ctrl Pts',(88.9472100964468,-3.97612241986335,0.908324667310112));
#10265=CARTESIAN_POINT('Ctrl Pts',(89.1146994034658,-2.92868745976694,-2.83855473126922));
#10266=CARTESIAN_POINT('Ctrl Pts',(89.2821887104848,0.783630603844815,-4.00256496199248));
#10267=CARTESIAN_POINT('Ctrl Pts',(89.4496780175041,3.78290434825481,-1.52454514234403));
#10268=CARTESIAN_POINT('Ctrl Pts',(89.617167324523,3.34002251362371,2.34069494173511));
#10269=CARTESIAN_POINT('Ctrl Pts',(89.7846566315421,-0.142026075882665,
4.07608044406827));
#10270=CARTESIAN_POINT('Ctrl Pts',(89.9521459385613,-3.49484172472506,2.10254239453794));
#10271=CARTESIAN_POINT('Ctrl Pts',(90.1196352455803,-3.66761690021701,-1.78414951469506));
#10272=CARTESIAN_POINT('Ctrl Pts',(90.2871245525994,-0.503139312267169,
-4.04740089207182));
#10273=CARTESIAN_POINT('Ctrl Pts',(90.4546138596184,3.11915682019817,-2.62782494967201));
#10274=CARTESIAN_POINT('Ctrl Pts',(90.6221031666376,3.90325721534673,1.18287210965676));
#10275=CARTESIAN_POINT('Ctrl Pts',(90.7895924736566,1.13569003616573,3.91724532637939));
#10276=CARTESIAN_POINT('Ctrl Pts',(90.9570817806758,-2.66526874350121,3.08722304209177));
#10277=CARTESIAN_POINT('Ctrl Pts',(91.1245710876948,-4.04103555251424,-0.551938002996637));
#10278=CARTESIAN_POINT('Ctrl Pts',(91.2920603947139,-1.73976677466987,-3.68887676195947));
#10279=CARTESIAN_POINT('Ctrl Pts',(91.4595497017329,2.14455716630937,-3.46921914937233));
#10280=CARTESIAN_POINT('Ctrl Pts',(91.6270390087521,4.07749786226986,-0.0928331999917247));
#10281=CARTESIAN_POINT('Ctrl Pts',(91.7945283157711,2.30022356589825,3.36801906256575));
#10282=CARTESIAN_POINT('Ctrl Pts',(91.9620176227901,-1.57007609244514,3.76423939164203));
#10283=CARTESIAN_POINT('Ctrl Pts',(92.1295069298093,-4.0117323669719,0.735269001609787));
#10284=CARTESIAN_POINT('Ctrl Pts',(92.2969962368283,-2.8030039668561,-2.96270320029105));
#10285=CARTESIAN_POINT('Ctrl Pts',(92.4644855438474,0.956219515839858,-3.96491373724205));
#10286=CARTESIAN_POINT('Ctrl Pts',(92.6319748508664,3.84540632500671,-1.35920972607447));
#10287=CARTESIAN_POINT('Ctrl Pts',(92.7994641578857,3.2354660655269,2.48298752514876));
#10288=CARTESIAN_POINT('Ctrl Pts',(92.9669534649045,-0.318306494350339,
4.06641529905593));
#10289=CARTESIAN_POINT('Ctrl Pts',(93.1344427719238,-3.58283088643105,1.94860893891442));
#10290=CARTESIAN_POINT('Ctrl Pts',(93.3019320789429,-3.58648771117453,-1.94010317901695));
#10291=CARTESIAN_POINT('Ctrl Pts',(93.4694213859618,-0.328237396709569,
-4.06778848006447));
#10292=CARTESIAN_POINT('Ctrl Pts',(93.636910692981,3.23190355653151,-2.48533100535543));
#10293=CARTESIAN_POINT('Ctrl Pts',(93.7485702309937,3.6386515229067,0.0637281040906096));
#10294=CARTESIAN_POINT('Ctrl Pts',(93.8044,3.25944077490411,1.14408268708712));
#10295=CARTESIAN_POINT('Ctrl Pts',(76.2850399531387,-3.44974973462971,0.00177277111675968));
#10296=CARTESIAN_POINT('Ctrl Pts',(76.3185306587644,-3.44656540712918,-0.687240312073141));
#10297=CARTESIAN_POINT('Ctrl Pts',(76.3520213643902,-3.24661788589681,-1.37796575952235));
#10298=CARTESIAN_POINT('Ctrl Pts',(76.3855120700159,-2.86252649231483,-1.94365074249582));
#10299=CARTESIAN_POINT('Ctrl Pts',(76.4413418390223,-2.22223739179093,-2.88666049220702));
#10300=CARTESIAN_POINT('Ctrl Pts',(76.4971716080286,-1.07021892791049,-3.48218717629386));
#10301=CARTESIAN_POINT('Ctrl Pts',(76.553001377035,0.0693892623577064,-3.4593241148768));
#10302=CARTESIAN_POINT('Ctrl Pts',(76.6088311460414,1.20899745262591,-3.43646105345974));
#10303=CARTESIAN_POINT('Ctrl Pts',(76.6646609150477,2.33619536928186,-2.79520824653877));
#10304=CARTESIAN_POINT('Ctrl Pts',(76.7204906840541,2.93815838175754,-1.82729343571165));
#10305=CARTESIAN_POINT('Ctrl Pts',(76.7763204530604,3.54012139423322,-0.859378624884532));
#10306=CARTESIAN_POINT('Ctrl Pts',(76.8321502220668,3.61684950252863,0.435198189848744));
#10307=CARTESIAN_POINT('Ctrl Pts',(76.8879799910732,3.13343047312431,1.46744463563674));
#10308=CARTESIAN_POINT('Ctrl Pts',(76.9438097600795,2.65001144371999,2.49969108142474));
#10309=CARTESIAN_POINT('Ctrl Pts',(76.9996395290858,1.60644527661593,3.26960715826746));
#10310=CARTESIAN_POINT('Ctrl Pts',(77.0554692980922,0.477516896797672,3.42691490934628));
#10311=CARTESIAN_POINT('Ctrl Pts',(77.1112990670986,-0.651411483020579,
3.58422266042509));
#10312=CARTESIAN_POINT('Ctrl Pts',(77.167128836105,-1.86570207555302,3.12892208574002));
#10313=CARTESIAN_POINT('Ctrl Pts',(77.2229586051113,-2.6128997775073,2.26815531216383));
#10314=CARTESIAN_POINT('Ctrl Pts',(77.2630968322316,-3.15008973187288,1.64931606438856));
#10315=CARTESIAN_POINT('Ctrl Pts',(77.3032350593518,-3.44585150244158,0.820901869180171));
#10316=CARTESIAN_POINT('Ctrl Pts',(77.343373286472,-3.45282914603924,-0.00301189592616661));
#10317=CARTESIAN_POINT('Origin',(74.3334724012261,0.,0.));
#10318=CARTESIAN_POINT('',(73.2669448024522,0.,0.));
#10319=CARTESIAN_POINT('',(74.3334724012261,-1.775,-2.17374806848655E-16));
#10320=CARTESIAN_POINT('Origin',(84.65,0.,0.));
#10321=CARTESIAN_POINT('Origin',(94.2,0.,0.));
#10322=CARTESIAN_POINT('',(94.4,-4.05000000000002,4.9598195365468E-16));
#10323=CARTESIAN_POINT('',(94.2,-3.85,-4.71489017671731E-16));
#10324=CARTESIAN_POINT('Origin',(94.4,0.,0.));
#10325=CARTESIAN_POINT('Origin',(9.,6.94,2.5));
#10326=CARTESIAN_POINT('',(13.,7.53615286469164,2.5));
#10327=CARTESIAN_POINT('',(5.,7.53615286469164,2.5));
#10328=CARTESIAN_POINT('',(47.3,7.53615286469164,2.5));
#10329=CARTESIAN_POINT('',(13.,4.94,2.5));
#10330=CARTESIAN_POINT('',(13.,4.94,2.5));
#10331=CARTESIAN_POINT('',(5.,4.94,2.5));
#10332=CARTESIAN_POINT('',(5.,4.94,2.5));
#10333=CARTESIAN_POINT('',(5.,8.94,2.5));
#10334=CARTESIAN_POINT('Origin',(5.,8.94,0.));
#10335=CARTESIAN_POINT('',(5.,7.53615286469164,-2.5));
#10336=CARTESIAN_POINT('Origin',(5.,0.,0.));
#10337=CARTESIAN_POINT('',(5.,4.94,-2.5));
#10338=CARTESIAN_POINT('',(5.,4.94,0.));
#10339=CARTESIAN_POINT('',(5.,8.94,-2.5));
#10340=CARTESIAN_POINT('Origin',(9.,6.94,-2.5));
#10341=CARTESIAN_POINT('',(13.,7.53615286469164,-2.5));
#10342=CARTESIAN_POINT('',(47.3,7.53615286469164,-2.5));
#10343=CARTESIAN_POINT('',(13.,4.94,-2.5));
#10344=CARTESIAN_POINT('',(5.,4.94,-2.5));
#10345=CARTESIAN_POINT('',(13.,4.94,-2.5));
#10346=CARTESIAN_POINT('Origin',(13.,4.94,0.));
#10347=CARTESIAN_POINT('Origin',(13.,0.,0.));
#10348=CARTESIAN_POINT('',(13.,4.94,0.));
#10349=CARTESIAN_POINT('Origin',(5.,4.94,0.));
#10350=CARTESIAN_POINT('Origin',(56.,6.94,2.5));
#10351=CARTESIAN_POINT('',(60.,7.53615286469164,2.5));
#10352=CARTESIAN_POINT('',(52.,7.53615286469164,2.5));
#10353=CARTESIAN_POINT('',(47.3,7.53615286469164,2.5));
#10354=CARTESIAN_POINT('',(60.,4.94,2.5));
#10355=CARTESIAN_POINT('',(60.,4.94,2.5));
#10356=CARTESIAN_POINT('',(52.,4.94,2.5));
#10357=CARTESIAN_POINT('',(52.,4.94,2.5));
#10358=CARTESIAN_POINT('',(52.,8.94,2.5));
#10359=CARTESIAN_POINT('Origin',(52.,8.94,0.));
#10360=CARTESIAN_POINT('',(52.,7.53615286469164,-2.5));
#10361=CARTESIAN_POINT('Origin',(52.,0.,0.));
#10362=CARTESIAN_POINT('',(52.,4.94,-2.5));
#10363=CARTESIAN_POINT('',(52.,4.94,0.));
#10364=CARTESIAN_POINT('',(52.,8.94,-2.5));
#10365=CARTESIAN_POINT('Origin',(56.,6.94,-2.5));
#10366=CARTESIAN_POINT('',(60.,7.53615286469164,-2.5));
#10367=CARTESIAN_POINT('',(47.3,7.53615286469164,-2.5));
#10368=CARTESIAN_POINT('',(60.,4.94,-2.5));
#10369=CARTESIAN_POINT('',(52.,4.94,-2.5));
#10370=CARTESIAN_POINT('',(60.,4.94,-2.5));
#10371=CARTESIAN_POINT('Origin',(60.,4.94,0.));
#10372=CARTESIAN_POINT('Origin',(60.,0.,0.));
#10373=CARTESIAN_POINT('',(60.,4.94,0.));
#10374=CARTESIAN_POINT('Origin',(52.,4.94,0.));
#10375=CARTESIAN_POINT('Origin',(73.6,7.6,0.));
#10376=CARTESIAN_POINT('',(73.6,-7.94,-9.72369558522999E-16));
#10377=CARTESIAN_POINT('Origin',(73.6,0.,0.));
#10378=CARTESIAN_POINT('',(73.6,-7.6,-9.30731567351989E-16));
#10379=CARTESIAN_POINT('Origin',(73.6,0.,0.));
#10380=CARTESIAN_POINT('Origin',(73.05,0.,0.));
#10381=CARTESIAN_POINT('',(72.5,-7.6,-9.30731567351989E-16));
#10382=CARTESIAN_POINT('Origin',(72.5,0.,0.));
#10383=CARTESIAN_POINT('',(73.05,-7.6,-9.30731567351989E-16));
#10384=CARTESIAN_POINT('Origin',(72.5,8.44,0.));
#10385=CARTESIAN_POINT('',(72.5,-7.94,9.72369558522999E-16));
#10386=CARTESIAN_POINT('Origin',(72.5,0.,0.));
#10387=CARTESIAN_POINT('Origin',(47.3,0.,0.));
#10388=CARTESIAN_POINT('',(3.,-7.94,-9.72369558522999E-16));
#10389=CARTESIAN_POINT('',(47.3,-7.94,-9.72369558522999E-16));
#10390=CARTESIAN_POINT('Origin',(3.,0.,0.));
#10391=CARTESIAN_POINT('Origin',(3.,7.6,0.));
#10392=CARTESIAN_POINT('',(3.,-7.6,-9.30731567351989E-16));
#10393=CARTESIAN_POINT('Origin',(3.,0.,0.));
#10394=CARTESIAN_POINT('Origin',(2.45,0.,0.));
#10395=CARTESIAN_POINT('',(1.9,-7.6,-9.30731567351989E-16));
#10396=CARTESIAN_POINT('Origin',(1.9,0.,0.));
#10397=CARTESIAN_POINT('',(2.45,-7.6,-9.30731567351989E-16));
#10398=CARTESIAN_POINT('Origin',(1.9,8.44,0.));
#10399=CARTESIAN_POINT('',(1.9,-7.94,9.72369558522999E-16));
#10400=CARTESIAN_POINT('Origin',(1.9,0.,0.));
#10401=CARTESIAN_POINT('Origin',(47.3,0.,0.));
#10402=CARTESIAN_POINT('',(0.999999999999996,-7.94,-9.72369558522999E-16));
#10403=CARTESIAN_POINT('',(47.3,-7.94,-9.72369558522999E-16));
#10404=CARTESIAN_POINT('Origin',(0.999999999999996,0.,0.));
#10405=CARTESIAN_POINT('Origin',(0.5,7.44,0.));
#10406=CARTESIAN_POINT('',(0.5,-7.44000000000001,-9.11137218565632E-16));
#10407=CARTESIAN_POINT('Origin',(0.500000000000007,0.,0.));
#10408=CARTESIAN_POINT('Origin',(0.749999999999993,0.,0.));
#10409=CARTESIAN_POINT('',(0.749999999999993,-7.69,-9.41753388544315E-16));
#10410=CARTESIAN_POINT('Origin',(47.3,0.,0.));
#10411=CARTESIAN_POINT('',(93.6,-7.94,-9.72369558522999E-16));
#10412=CARTESIAN_POINT('Origin',(93.6,0.,0.));
#10413=CARTESIAN_POINT('',(47.3,-7.94,-9.72369558522999E-16));
#10414=CARTESIAN_POINT('Origin',(94.,0.,0.));
#10415=CARTESIAN_POINT('',(94.4,-7.14,-8.7439781459121E-16));
#10416=CARTESIAN_POINT('Origin',(94.4,0.,0.));
#10417=CARTESIAN_POINT('',(94.,-7.54,-9.23383686557104E-16));
#10418=CARTESIAN_POINT('Origin',(94.4,0.,0.));
#10419=CARTESIAN_POINT('',(0.,0.,0.));
#10420=CARTESIAN_POINT('Origin',(0.5,0.,0.));
#10421=CARTESIAN_POINT('',(0.,56.4788841358559,2.5));
#10422=CARTESIAN_POINT('',(0.179907800166174,56.0951492439243,2.48301423187597));
#10423=CARTESIAN_POINT('Origin',(0.5,56.4788841358559,2.50000000000001));
#10424=CARTESIAN_POINT('',(0.17990780016617,56.0951492439243,-2.48301423187597));
#10425=CARTESIAN_POINT('Origin',(0.17990780016776,0.,-8.59550148320605E-15));
#10426=CARTESIAN_POINT('',(0.,56.4788841358559,-2.5));
#10427=CARTESIAN_POINT('Origin',(0.5,56.4788841358559,-2.49999999999988));
#10428=CARTESIAN_POINT('Origin',(0.,0.,0.));
#10429=CARTESIAN_POINT('Origin',(0.5,56.4788841358559,-2.5));
#10430=CARTESIAN_POINT('',(0.499999999997957,56.4788841358593,-2.));
#10431=CARTESIAN_POINT('Ctrl Pts',(0.179907800164864,56.095149243924,-2.48301423187597));
#10432=CARTESIAN_POINT('Ctrl Pts',(0.182694641762887,56.0984901824412,-2.3550199649901));
#10433=CARTESIAN_POINT('Ctrl Pts',(0.254541365578152,56.1846219120289,-2.1035560356539));
#10434=CARTESIAN_POINT('Ctrl Pts',(0.417965393799912,56.380538906701,-2.));
#10435=CARTESIAN_POINT('Ctrl Pts',(0.499999999997104,56.4788841358583,-2.));
#10436=CARTESIAN_POINT('Origin',(0.5,56.4788841358559,-2.5));
#10437=CARTESIAN_POINT('Origin',(0.5,56.4788841358559,2.5));
#10438=CARTESIAN_POINT('',(0.499999999997957,56.4788841358593,2.));
#10439=CARTESIAN_POINT('Ctrl Pts',(0.499999999997116,56.4788841358583,2.));
#10440=CARTESIAN_POINT('Ctrl Pts',(0.417965393799925,56.380538906701,2.));
#10441=CARTESIAN_POINT('Ctrl Pts',(0.254541365578165,56.1846219120289,2.1035560356539));
#10442=CARTESIAN_POINT('Ctrl Pts',(0.1826946417629,56.0984901824412,2.3550199649901));
#10443=CARTESIAN_POINT('Ctrl Pts',(0.179907800164876,56.095149243924,2.48301423187597));
#10444=CARTESIAN_POINT('Origin',(0.5,56.4788841358559,2.5));
#10445=CARTESIAN_POINT('Ctrl Pts',(0.499999999997116,56.4788841358583,2.));
#10446=CARTESIAN_POINT('Ctrl Pts',(0.593634842898508,56.4007786951615,2.));
#10447=CARTESIAN_POINT('Ctrl Pts',(0.687269529957182,56.3226730676369,2.));
#10448=CARTESIAN_POINT('Ctrl Pts',(0.780904059217746,56.2445672509427,2.));
#10449=CARTESIAN_POINT('Ctrl Pts',(0.417965393799925,56.380538906701,2.));
#10450=CARTESIAN_POINT('Ctrl Pts',(0.511602632292953,56.3024366043021,2.00000011921147));
#10451=CARTESIAN_POINT('Ctrl Pts',(0.605239657990774,56.2243340470848,1.99999987982881));
#10452=CARTESIAN_POINT('Ctrl Pts',(0.698876602273683,56.1462313952731,2.));
#10453=CARTESIAN_POINT('Ctrl Pts',(0.254541365578165,56.1846219120289,2.1035560356539));
#10454=CARTESIAN_POINT('Ctrl Pts',(0.348183189883171,56.1065256357554,2.10354935262451));
#10455=CARTESIAN_POINT('Ctrl Pts',(0.441824994766503,56.0284293435913,2.10354276030279));
#10456=CARTESIAN_POINT('Ctrl Pts',(0.53546656209897,55.9503327690787,2.1035360223157));
#10457=CARTESIAN_POINT('Ctrl Pts',(0.1826946417629,56.0984901824412,2.3550199649901));
#10458=CARTESIAN_POINT('Ctrl Pts',(0.276333332478559,56.0203903852816,2.35500062661495));
#10459=CARTESIAN_POINT('Ctrl Pts',(0.369971635899614,55.9422901242085,2.35498122632127));
#10460=CARTESIAN_POINT('Ctrl Pts',(0.463610044339371,55.8641900014912,2.35496172772305));
#10461=CARTESIAN_POINT('Ctrl Pts',(0.179907800164876,56.095149243924,2.48301423187597));
#10462=CARTESIAN_POINT('Ctrl Pts',(0.273542643066269,56.0170448409568,2.4829907879535));
#10463=CARTESIAN_POINT('Ctrl Pts',(0.367177330124943,55.9389402576093,2.48296724699913));
#10464=CARTESIAN_POINT('Ctrl Pts',(0.460811859385507,55.8608354916477,2.48294360779847));
#10465=CARTESIAN_POINT('',(0.780904059217604,56.2445672509427,2.));
#10466=CARTESIAN_POINT('Ctrl Pts',(0.499999999997116,56.4788841358583,2.));
#10467=CARTESIAN_POINT('Ctrl Pts',(0.593634842898508,56.4007786951615,2.));
#10468=CARTESIAN_POINT('Ctrl Pts',(0.687269529957182,56.3226730676369,2.));
#10469=CARTESIAN_POINT('Ctrl Pts',(0.780904059217746,56.2445672509427,2.));
#10470=CARTESIAN_POINT('',(0.460811859385445,55.8608354916477,2.48294360779849));
#10471=CARTESIAN_POINT('Origin',(0.7809040592178,56.2445672509427,2.5));
#10472=CARTESIAN_POINT('Ctrl Pts',(0.460811859385507,55.8608354916477,2.48294360779847));
#10473=CARTESIAN_POINT('Ctrl Pts',(0.367177330124943,55.9389402576093,2.48296724699913));
#10474=CARTESIAN_POINT('Ctrl Pts',(0.273542643066269,56.0170448409568,2.4829907879535));
#10475=CARTESIAN_POINT('Ctrl Pts',(0.179907800164876,56.095149243924,2.48301423187597));
#10476=CARTESIAN_POINT('Origin',(0.5,57.025,2.5));
#10477=CARTESIAN_POINT('',(0.,56.8978458123627,2.5));
#10478=CARTESIAN_POINT('',(0.,57.025,2.5));
#10479=CARTESIAN_POINT('',(0.500000000000237,56.8978458123627,2.));
#10480=CARTESIAN_POINT('Origin',(0.5,56.8978458123627,2.5));
#10481=CARTESIAN_POINT('',(0.5,57.025,2.));
#10482=CARTESIAN_POINT('Origin',(0.,57.3,0.));
#10483=CARTESIAN_POINT('',(0.,56.8978458123625,-2.49999999999977));
#10484=CARTESIAN_POINT('',(0.,57.025,-2.5));
#10485=CARTESIAN_POINT('Ctrl Pts',(0.,56.8978458123625,2.49999999999978));
#10486=CARTESIAN_POINT('Ctrl Pts',(0.,56.5290913566253,10.8925336660656));
#10487=CARTESIAN_POINT('Ctrl Pts',(0.,52.0239399392849,27.5104427981014));
#10488=CARTESIAN_POINT('Ctrl Pts',(0.,37.0895128901808,44.9505513524534));
#10489=CARTESIAN_POINT('Ctrl Pts',(0.,19.6413066333793,54.3407718417784));
#10490=CARTESIAN_POINT('Ctrl Pts',(0.,2.98972976337264,57.7126473424414));
#10491=CARTESIAN_POINT('Ctrl Pts',(0.,-13.9100795010715,56.0762889490297));
#10492=CARTESIAN_POINT('Ctrl Pts',(0.,-34.8726547481504,47.4775611101652));
#10493=CARTESIAN_POINT('Ctrl Pts',(0.,-48.6578954952714,32.3601597542925));
#10494=CARTESIAN_POINT('Ctrl Pts',(0.,-54.6754985459398,16.615078371656));
#10495=CARTESIAN_POINT('Ctrl Pts',(0.,-58.4322800872165,0.182637285551057));
#10496=CARTESIAN_POINT('Ctrl Pts',(0.,-55.3972091422166,-20.0478023034309));
#10497=CARTESIAN_POINT('Ctrl Pts',(0.,-42.7587268357465,-38.8566003856648));
#10498=CARTESIAN_POINT('Ctrl Pts',(0.,-29.6277979733952,-49.6176180623964));
#10499=CARTESIAN_POINT('Ctrl Pts',(0.,-13.9134722149986,-56.083084294608));
#10500=CARTESIAN_POINT('Ctrl Pts',(0.,2.99163137042858,-57.710045079662));
#10501=CARTESIAN_POINT('Ctrl Pts',(0.,19.6409629692718,-54.3421091676748));
#10502=CARTESIAN_POINT('Ctrl Pts',(0.,37.0902013849514,-44.9493511994273));
#10503=CARTESIAN_POINT('Ctrl Pts',(0.,52.0238383479187,-27.5106172571882));
#10504=CARTESIAN_POINT('Ctrl Pts',(0.,56.5290913566252,-10.8925336660656));
#10505=CARTESIAN_POINT('Ctrl Pts',(0.,56.8978458123625,-2.49999999999977));
#10506=CARTESIAN_POINT('Ctrl Pts',(0.772591931467417,55.7451294709179,2.47780062126729));
#10507=CARTESIAN_POINT('Ctrl Pts',(0.772591931467417,55.379709551606,10.6989547118962));
#10508=CARTESIAN_POINT('Ctrl Pts',(0.772591931467379,50.9581493156086,26.9764013787265));
#10509=CARTESIAN_POINT('Ctrl Pts',(0.772591931467366,36.3233521724092,44.0527896931361));
#10510=CARTESIAN_POINT('Ctrl Pts',(0.77259193146737,19.2256187449638,53.2486164943009));
#10511=CARTESIAN_POINT('Ctrl Pts',(0.772591931467382,2.91685365030647,56.5415921245837));
#10512=CARTESIAN_POINT('Ctrl Pts',(0.772591931467353,-13.6471652991449,
54.9460594777695));
#10513=CARTESIAN_POINT('Ctrl Pts',(0.77259193146742,-29.0305558907579,48.6064856663137));
#10514=CARTESIAN_POINT('Ctrl Pts',(0.772591931467399,-41.9074799864638,
38.0671554541429));
#10515=CARTESIAN_POINT('Ctrl Pts',(0.772591931467406,-51.1637806560337,
24.240464632067));
#10516=CARTESIAN_POINT('Ctrl Pts',(0.772591931467356,-56.0014365376947,
8.31948037804371));
#10517=CARTESIAN_POINT('Ctrl Pts',(0.772591931467423,-56.0009380440498,
-8.31968241557478));
#10518=CARTESIAN_POINT('Ctrl Pts',(0.772591931467387,-51.1640653905075,
-24.2409304612857));
#10519=CARTESIAN_POINT('Ctrl Pts',(0.772591931467385,-41.9071399938438,
-38.0674064524271));
#10520=CARTESIAN_POINT('Ctrl Pts',(0.772591931467373,-29.0304426638128,
-48.6065966625385));
#10521=CARTESIAN_POINT('Ctrl Pts',(0.772591931467365,-13.6468152705721,
-54.9457263658574));
#10522=CARTESIAN_POINT('Ctrl Pts',(0.772591931467323,2.91739716720752,-56.5422576232864));
#10523=CARTESIAN_POINT('Ctrl Pts',(0.772591931467349,19.2260068136787,-53.2483487259477));
#10524=CARTESIAN_POINT('Ctrl Pts',(0.772591931467411,36.3234077815813,-44.0527282308743));
#10525=CARTESIAN_POINT('Ctrl Pts',(0.772591931467395,50.9584317787812,-26.975898664924));
#10526=CARTESIAN_POINT('Ctrl Pts',(0.772591931467383,55.379709551606,-10.6989547118962));
#10527=CARTESIAN_POINT('Ctrl Pts',(0.772591931467384,55.7451294709179,-2.47780062126731));
#10528=CARTESIAN_POINT('Ctrl Pts',(0.659588674014702,55.747006472314,2.47788405160945));
#10529=CARTESIAN_POINT('Ctrl Pts',(0.659588674014702,55.3815762057712,10.6992709324469));
#10530=CARTESIAN_POINT('Ctrl Pts',(0.659588674014685,50.9598613650699,26.9773401036556));
#10531=CARTESIAN_POINT('Ctrl Pts',(0.659588674014669,36.3245761421025,44.0542605993868));
#10532=CARTESIAN_POINT('Ctrl Pts',(0.65958867401467,19.2262615067636,53.2504137911799));
#10533=CARTESIAN_POINT('Ctrl Pts',(0.659588674014682,2.91695282870238,56.543493263952));
#10534=CARTESIAN_POINT('Ctrl Pts',(0.659588674014657,-13.647622959522,54.9479091625884));
#10535=CARTESIAN_POINT('Ctrl Pts',(0.659588674014704,-29.0315351701335,
48.6081203793897));
#10536=CARTESIAN_POINT('Ctrl Pts',(0.659588674014695,-41.9088877796823,
38.0684377192795));
#10537=CARTESIAN_POINT('Ctrl Pts',(0.659588674014705,-51.1655032091182,
24.241282493667));
#10538=CARTESIAN_POINT('Ctrl Pts',(0.65958867401464,-56.0033201731021,8.31975571353977));
#10539=CARTESIAN_POINT('Ctrl Pts',(0.659588674014727,-56.0028236846315,
-8.31996139839591));
#10540=CARTESIAN_POINT('Ctrl Pts',(0.659588674014686,-51.1657866585822,
-24.2417444733812));
#10541=CARTESIAN_POINT('Ctrl Pts',(0.659588674014683,-41.9085495140753,
-38.0686899407466));
#10542=CARTESIAN_POINT('Ctrl Pts',(0.659588674014673,-29.0314210013225,
-48.608229623483));
#10543=CARTESIAN_POINT('Ctrl Pts',(0.659588674014657,-13.6472763990038,
-54.9475778572917));
#10544=CARTESIAN_POINT('Ctrl Pts',(0.659588674014636,2.91749931213322,-56.5441560813714));
#10545=CARTESIAN_POINT('Ctrl Pts',(0.659588674014654,19.2266538416122,-53.2501458099667));
#10546=CARTESIAN_POINT('Ctrl Pts',(0.659588674014694,36.3246254700402,-44.0542012209058));
#10547=CARTESIAN_POINT('Ctrl Pts',(0.659588674014703,50.960147755993,-26.9768360225067));
#10548=CARTESIAN_POINT('Ctrl Pts',(0.659588674014674,55.3815762057712,-10.6992709324469));
#10549=CARTESIAN_POINT('Ctrl Pts',(0.659588674014674,55.747006472314,-2.47788405160947));
#10550=CARTESIAN_POINT('Ctrl Pts',(0.547635364780324,55.788553938233,2.47973078401178));
#10551=CARTESIAN_POINT('Ctrl Pts',(0.547635364780324,55.4228512437384,10.7072467017526));
#10552=CARTESIAN_POINT('Ctrl Pts',(0.547635364780334,50.9978411885347,26.9974447290012));
#10553=CARTESIAN_POINT('Ctrl Pts',(0.547635364780309,36.3516483050864,44.0870941184864));
#10554=CARTESIAN_POINT('Ctrl Pts',(0.547635364780313,19.2405907536628,53.2901004080723));
#10555=CARTESIAN_POINT('Ctrl Pts',(0.547635364780321,2.91912675454844,56.5856344470053));
#10556=CARTESIAN_POINT('Ctrl Pts',(0.547635364780301,-13.6577944162708,
54.9888610887901));
#10557=CARTESIAN_POINT('Ctrl Pts',(0.547635364780325,-29.0531718969856,
48.6443474096255));
#10558=CARTESIAN_POINT('Ctrl Pts',(0.54763536478033,-41.9401220193493,38.0968095746887));
#10559=CARTESIAN_POINT('Ctrl Pts',(0.547635364780343,-51.2036361521209,
24.2593491172253));
#10560=CARTESIAN_POINT('Ctrl Pts',(0.547635364780263,-56.045058745482,8.32595650201345));
#10561=CARTESIAN_POINT('Ctrl Pts',(0.547635364780371,-56.044561806521,-8.32616219528814));
#10562=CARTESIAN_POINT('Ctrl Pts',(0.547635364780327,-51.2039198643548,
-24.2598115950628));
#10563=CARTESIAN_POINT('Ctrl Pts',(0.54763536478032,-41.9397834324552,-38.0970619357924));
#10564=CARTESIAN_POINT('Ctrl Pts',(0.547635364780315,-29.0530576804163,
-48.6444568050123));
#10565=CARTESIAN_POINT('Ctrl Pts',(0.547635364780284,-13.6574474589847,
-54.9885294642351));
#10566=CARTESIAN_POINT('Ctrl Pts',(0.547635364780292,2.91967352794025,-56.5862978660074));
#10567=CARTESIAN_POINT('Ctrl Pts',(0.547635364780297,19.2409832116612,-53.2898322352485));
#10568=CARTESIAN_POINT('Ctrl Pts',(0.547635364780317,36.3516979198253,-44.0870346127446));
#10569=CARTESIAN_POINT('Ctrl Pts',(0.547635364780352,50.9981276369736,-26.9969403259078));
#10570=CARTESIAN_POINT('Ctrl Pts',(0.547635364780302,55.4228512437384,-10.7072467017526));
#10571=CARTESIAN_POINT('Ctrl Pts',(0.547635364780302,55.788553938233,-2.4797307840118));
#10572=CARTESIAN_POINT('Ctrl Pts',(0.460811859385443,55.8608354916477,2.48294360779849));
#10573=CARTESIAN_POINT('Ctrl Pts',(0.460811859385443,55.4946570973774,10.7211617367507));
#10574=CARTESIAN_POINT('Ctrl Pts',(0.460811859385469,51.0639193575303,27.0323942894394));
#10575=CARTESIAN_POINT('Ctrl Pts',(0.46081185938544,36.3987458539618,44.1442267934859));
#10576=CARTESIAN_POINT('Ctrl Pts',(0.460811859385444,19.2655239324154,53.3591406886548));
#10577=CARTESIAN_POINT('Ctrl Pts',(0.46081185938545,2.92290794656755,56.6589513036287));
#10578=CARTESIAN_POINT('Ctrl Pts',(0.460811859385435,-13.6754917055233,
55.0601069283235));
#10579=CARTESIAN_POINT('Ctrl Pts',(0.460811859385444,-29.09081245727,48.7073745348389));
#10580=CARTESIAN_POINT('Ctrl Pts',(0.460811859385456,-41.9944642269539,
38.1461686185199));
#10581=CARTESIAN_POINT('Ctrl Pts',(0.460811859385471,-51.2699775116405,
24.290778762285));
#10582=CARTESIAN_POINT('Ctrl Pts',(0.460811859385381,-56.1176745559473,
8.33674850493155));
#10583=CARTESIAN_POINT('Ctrl Pts',(0.460811859385504,-56.1171750276162,
-8.33695096181688));
#10584=CARTESIAN_POINT('Ctrl Pts',(0.460811859385457,-51.2702628371164,
-24.2912455583908));
#10585=CARTESIAN_POINT('Ctrl Pts',(0.460811859385448,-41.9941235286365,
-38.1464201377825));
#10586=CARTESIAN_POINT('Ctrl Pts',(0.460811859385444,-29.0906989953083,
-48.7074857614504));
#10587=CARTESIAN_POINT('Ctrl Pts',(0.460811859385409,-13.6751409504222,
-55.0597731249957));
#10588=CARTESIAN_POINT('Ctrl Pts',(0.460811859385431,2.92345259160619,-56.6596181836576));
#10589=CARTESIAN_POINT('Ctrl Pts',(0.46081185938543,19.2659128066157,-53.3588723645147));
#10590=CARTESIAN_POINT('Ctrl Pts',(0.460811859385435,36.3988015785576,-44.1441652036514));
#10591=CARTESIAN_POINT('Ctrl Pts',(0.460811859385486,51.0642024069907,-27.0318905321913));
#10592=CARTESIAN_POINT('Ctrl Pts',(0.460811859385425,55.4946570973774,-10.7211617367508));
#10593=CARTESIAN_POINT('Ctrl Pts',(0.460811859385425,55.8608354916477,-2.48294360779851));
#10594=CARTESIAN_POINT('',(0.772591931467425,55.7451294709179,-2.47780062126728));
#10595=CARTESIAN_POINT('',(0.460811859385434,55.8608354916477,-2.48294360779851));
#10596=CARTESIAN_POINT('Origin',(0.780904059217663,56.2445672509427,-2.50000000000004));
#10597=CARTESIAN_POINT('Ctrl Pts',(0.460811859385425,55.8608354916477,-2.48294360779851));
#10598=CARTESIAN_POINT('Ctrl Pts',(0.460811859385425,55.4946570973774,-10.7211617367508));
#10599=CARTESIAN_POINT('Ctrl Pts',(0.460811859385486,51.0642024069907,-27.0318905321913));
#10600=CARTESIAN_POINT('Ctrl Pts',(0.460811859385435,36.3988015785576,-44.1441652036514));
#10601=CARTESIAN_POINT('Ctrl Pts',(0.46081185938543,19.2659128066157,-53.3588723645147));
#10602=CARTESIAN_POINT('Ctrl Pts',(0.460811859385431,2.92345259160619,-56.6596181836576));
#10603=CARTESIAN_POINT('Ctrl Pts',(0.460811859385409,-13.6751409504222,
-55.0597731249957));
#10604=CARTESIAN_POINT('Ctrl Pts',(0.460811859385444,-29.0906989953083,
-48.7074857614504));
#10605=CARTESIAN_POINT('Ctrl Pts',(0.460811859385448,-41.9941235286365,
-38.1464201377825));
#10606=CARTESIAN_POINT('Ctrl Pts',(0.460811859385457,-51.2702628371164,
-24.2912455583908));
#10607=CARTESIAN_POINT('Ctrl Pts',(0.460811859385504,-56.1171750276162,
-8.33695096181688));
#10608=CARTESIAN_POINT('Ctrl Pts',(0.460811859385381,-56.1176745559473,
8.33674850493155));
#10609=CARTESIAN_POINT('Ctrl Pts',(0.460811859385471,-51.2699775116405,
24.290778762285));
#10610=CARTESIAN_POINT('Ctrl Pts',(0.460811859385456,-41.9944642269539,
38.1461686185199));
#10611=CARTESIAN_POINT('Ctrl Pts',(0.460811859385444,-29.09081245727,48.7073745348389));
#10612=CARTESIAN_POINT('Ctrl Pts',(0.460811859385435,-13.6754917055233,
55.0601069283235));
#10613=CARTESIAN_POINT('Ctrl Pts',(0.46081185938545,2.92290794656755,56.6589513036287));
#10614=CARTESIAN_POINT('Ctrl Pts',(0.460811859385444,19.2655239324154,53.3591406886548));
#10615=CARTESIAN_POINT('Ctrl Pts',(0.46081185938544,36.3987458539618,44.1442267934859));
#10616=CARTESIAN_POINT('Ctrl Pts',(0.460811859385469,51.0639193575303,27.0323942894394));
#10617=CARTESIAN_POINT('Ctrl Pts',(0.460811859385443,55.4946570973774,10.7211617367507));
#10618=CARTESIAN_POINT('Ctrl Pts',(0.460811859385443,55.8608354916477,2.48294360779849));
#10619=CARTESIAN_POINT('',(0.772591931467348,55.7451294709179,2.47780062126728));
#10620=CARTESIAN_POINT('Origin',(0.780904059217683,56.2445672509427,2.50000000000002));
#10621=CARTESIAN_POINT('Ctrl Pts',(0.772591931467417,55.7451294709179,2.47780062126729));
#10622=CARTESIAN_POINT('Ctrl Pts',(0.772591931467417,55.379709551606,10.6989547118962));
#10623=CARTESIAN_POINT('Ctrl Pts',(0.772591931467379,50.9581493156086,26.9764013787265));
#10624=CARTESIAN_POINT('Ctrl Pts',(0.772591931467366,36.3233521724092,44.0527896931361));
#10625=CARTESIAN_POINT('Ctrl Pts',(0.77259193146737,19.2256187449638,53.2486164943009));
#10626=CARTESIAN_POINT('Ctrl Pts',(0.772591931467382,2.91685365030647,56.5415921245837));
#10627=CARTESIAN_POINT('Ctrl Pts',(0.772591931467353,-13.6471652991449,
54.9460594777695));
#10628=CARTESIAN_POINT('Ctrl Pts',(0.77259193146742,-29.0305558907579,48.6064856663137));
#10629=CARTESIAN_POINT('Ctrl Pts',(0.772591931467399,-41.9074799864638,
38.0671554541429));
#10630=CARTESIAN_POINT('Ctrl Pts',(0.772591931467406,-51.1637806560337,
24.240464632067));
#10631=CARTESIAN_POINT('Ctrl Pts',(0.772591931467356,-56.0014365376947,
8.31948037804371));
#10632=CARTESIAN_POINT('Ctrl Pts',(0.772591931467423,-56.0009380440498,
-8.31968241557478));
#10633=CARTESIAN_POINT('Ctrl Pts',(0.772591931467387,-51.1640653905075,
-24.2409304612857));
#10634=CARTESIAN_POINT('Ctrl Pts',(0.772591931467385,-41.9071399938438,
-38.0674064524271));
#10635=CARTESIAN_POINT('Ctrl Pts',(0.772591931467373,-29.0304426638128,
-48.6065966625385));
#10636=CARTESIAN_POINT('Ctrl Pts',(0.772591931467365,-13.6468152705721,
-54.9457263658574));
#10637=CARTESIAN_POINT('Ctrl Pts',(0.772591931467323,2.91739716720752,-56.5422576232864));
#10638=CARTESIAN_POINT('Ctrl Pts',(0.772591931467349,19.2260068136787,-53.2483487259477));
#10639=CARTESIAN_POINT('Ctrl Pts',(0.772591931467411,36.3234077815813,-44.0527282308743));
#10640=CARTESIAN_POINT('Ctrl Pts',(0.772591931467395,50.9584317787812,-26.975898664924));
#10641=CARTESIAN_POINT('Ctrl Pts',(0.772591931467383,55.379709551606,-10.6989547118962));
#10642=CARTESIAN_POINT('Ctrl Pts',(0.772591931467384,55.7451294709179,-2.47780062126731));
#10643=CARTESIAN_POINT('Origin',(0.780904059217543,56.2445672509427,-2.49999999999999));
#10644=CARTESIAN_POINT('',(0.780904059217487,56.2445672509427,-2.));
#10645=CARTESIAN_POINT('Origin',(0.780904059217543,56.2445672509427,-2.49999999999999));
#10646=CARTESIAN_POINT('Origin',(0.780904059217543,56.2445672509427,-2.49999999999999));
#10647=CARTESIAN_POINT('Origin',(0.7809040592178,56.2445672509427,2.5));
#10648=CARTESIAN_POINT('Origin',(0.7809040592178,56.2445672509427,2.5));
#10649=CARTESIAN_POINT('Ctrl Pts',(0.179907800164864,56.095149243924,-2.48301423187597));
#10650=CARTESIAN_POINT('Ctrl Pts',(0.273542643066175,56.0170448409569,-2.4829907879535));
#10651=CARTESIAN_POINT('Ctrl Pts',(0.367177330124766,55.9389402576095,-2.48296724699913));
#10652=CARTESIAN_POINT('Ctrl Pts',(0.460811859385246,55.8608354916479,-2.48294360779847));
#10653=CARTESIAN_POINT('Ctrl Pts',(0.182694641762887,56.0984901824412,-2.3550199649901));
#10654=CARTESIAN_POINT('Ctrl Pts',(0.276333332478466,56.0203903852817,-2.35500062661495));
#10655=CARTESIAN_POINT('Ctrl Pts',(0.369971635899436,55.9422901242086,-2.35498122632127));
#10656=CARTESIAN_POINT('Ctrl Pts',(0.46361004433911,55.8641900014914,-2.35496172772305));
#10657=CARTESIAN_POINT('Ctrl Pts',(0.254541365578152,56.1846219120289,-2.1035560356539));
#10658=CARTESIAN_POINT('Ctrl Pts',(0.348183189883077,56.1065256357555,-2.10354935262451));
#10659=CARTESIAN_POINT('Ctrl Pts',(0.441824994766326,56.0284293435915,-2.10354276030279));
#10660=CARTESIAN_POINT('Ctrl Pts',(0.535466562098709,55.9503327690789,-2.1035360223157));
#10661=CARTESIAN_POINT('Ctrl Pts',(0.417965393799912,56.380538906701,-2.));
#10662=CARTESIAN_POINT('Ctrl Pts',(0.51160263229286,56.3024366043021,-2.00000011921147));
#10663=CARTESIAN_POINT('Ctrl Pts',(0.605239657990597,56.224334047085,-1.99999987982882));
#10664=CARTESIAN_POINT('Ctrl Pts',(0.698876602273422,56.1462313952734,-2.00000000000001));
#10665=CARTESIAN_POINT('Ctrl Pts',(0.499999999997104,56.4788841358583,-2.));
#10666=CARTESIAN_POINT('Ctrl Pts',(0.593634842898415,56.4007786951616,-2.));
#10667=CARTESIAN_POINT('Ctrl Pts',(0.687269529957005,56.3226730676371,-2.00000000000001));
#10668=CARTESIAN_POINT('Ctrl Pts',(0.780904059217486,56.2445672509429,-2.00000000000001));
#10669=CARTESIAN_POINT('Ctrl Pts',(0.179907800164864,56.095149243924,-2.48301423187597));
#10670=CARTESIAN_POINT('Ctrl Pts',(0.273542643066175,56.0170448409569,-2.4829907879535));
#10671=CARTESIAN_POINT('Ctrl Pts',(0.367177330124766,55.9389402576095,-2.48296724699913));
#10672=CARTESIAN_POINT('Ctrl Pts',(0.460811859385246,55.8608354916479,-2.48294360779847));
#10673=CARTESIAN_POINT('Ctrl Pts',(0.780904059217486,56.2445672509429,-2.00000000000001));
#10674=CARTESIAN_POINT('Ctrl Pts',(0.687269529957005,56.3226730676371,-2.00000000000001));
#10675=CARTESIAN_POINT('Ctrl Pts',(0.593634842898415,56.4007786951616,-2.));
#10676=CARTESIAN_POINT('Ctrl Pts',(0.499999999997104,56.4788841358583,-2.));
#10677=CARTESIAN_POINT('Ctrl Pts',(3.30000000000011,55.3431808226541,-2.));
#10678=CARTESIAN_POINT('Ctrl Pts',(2.61488947773062,55.9545258328107,-2.));
#10679=CARTESIAN_POINT('Ctrl Pts',(1.68855421348719,56.2382465200534,-2.));
#10680=CARTESIAN_POINT('Ctrl Pts',(0.780904059217557,56.2445672509427,-2.));
#10681=CARTESIAN_POINT('Ctrl Pts',(3.12847993397321,55.1464989588649,-1.99359023604657));
#10682=CARTESIAN_POINT('Ctrl Pts',(2.49435860108456,55.7131228937494,-1.99369822098603));
#10683=CARTESIAN_POINT('Ctrl Pts',(1.6423051555987,55.9779696257069,-1.99374127621725));
#10684=CARTESIAN_POINT('Ctrl Pts',(0.776592785321963,55.985522499928,-1.99373831640894));
#10685=CARTESIAN_POINT('Ctrl Pts',(2.97318977758963,54.9684279139248,-2.22195490734826));
#10686=CARTESIAN_POINT('Ctrl Pts',(2.38493152738063,55.4942042697613,-2.219584961608));
#10687=CARTESIAN_POINT('Ctrl Pts',(1.60032112558294,55.7416794204833,-2.2186313537272));
#10688=CARTESIAN_POINT('Ctrl Pts',(0.772679250843375,55.750376093287,-2.21869746782962));
#10689=CARTESIAN_POINT('Ctrl Pts',(2.97156409628604,54.9665637470309,-2.4829871959822));
#10690=CARTESIAN_POINT('Ctrl Pts',(2.3824255311525,55.4902988970164,-2.47922636145333));
#10691=CARTESIAN_POINT('Ctrl Pts',(1.59937395537643,55.7362908562734,-2.47769302204319));
#10692=CARTESIAN_POINT('Ctrl Pts',(0.772591931467199,55.7451294709179,-2.47780062126726));
#10693=CARTESIAN_POINT('',(2.971564096286,54.9665637470309,-2.48298719598216));
#10694=CARTESIAN_POINT('Ctrl Pts',(0.772591931467199,55.7451294709179,-2.47780062126726));
#10695=CARTESIAN_POINT('Ctrl Pts',(1.59937395537643,55.7362908562734,-2.47769302204319));
#10696=CARTESIAN_POINT('Ctrl Pts',(2.3824255311525,55.4902988970164,-2.47922636145333));
#10697=CARTESIAN_POINT('Ctrl Pts',(2.97156409628604,54.9665637470309,-2.4829871959822));
#10698=CARTESIAN_POINT('',(2.8,55.359994587709,-2.09491355855718));
#10699=CARTESIAN_POINT('Ctrl Pts',(2.971564096286,54.9665637470309,-2.4829871959822));
#10700=CARTESIAN_POINT('Ctrl Pts',(2.97105810082493,54.9670227222473,-2.48226197818885));
#10701=CARTESIAN_POINT('Ctrl Pts',(2.97055313800993,54.9674828549434,-2.48153699974797));
#10702=CARTESIAN_POINT('Ctrl Pts',(2.97004920764725,54.9679441397298,-2.48081226422373));
#10703=CARTESIAN_POINT('Ctrl Pts',(2.95167041222309,54.9847676124758,-2.45438050514927));
#10704=CARTESIAN_POINT('Ctrl Pts',(2.9345112351927,55.003258903751,-2.42807817015696));
#10705=CARTESIAN_POINT('Ctrl Pts',(2.91866949298605,55.0232080767984,-2.4020995131002));
#10706=CARTESIAN_POINT('Ctrl Pts',(2.90322420614785,55.0426580019318,-2.37677099779685));
#10707=CARTESIAN_POINT('Ctrl Pts',(2.8890308989744,55.0634947711076,-2.35174970589681));
#10708=CARTESIAN_POINT('Ctrl Pts',(2.87621470782766,55.085540523235,-2.32724566770674));
#10709=CARTESIAN_POINT('Ctrl Pts',(2.86402565276861,55.1065075081544,-2.30394068830622));
#10710=CARTESIAN_POINT('Ctrl Pts',(2.85308218625054,55.1285688920359,-2.28110332092758));
#10711=CARTESIAN_POINT('Ctrl Pts',(2.8435260528693,55.1515737238906,-2.25894659880361));
#10712=CARTESIAN_POINT('Ctrl Pts',(2.84019421835236,55.1595945718394,-2.25122145217687));
#10713=CARTESIAN_POINT('Ctrl Pts',(2.83703135085799,55.1677300706399,-2.24357936415525));
#10714=CARTESIAN_POINT('Ctrl Pts',(2.83404451182727,55.1759736024566,-2.23603044811829));
#10715=CARTESIAN_POINT('Ctrl Pts',(2.82677792422061,55.1960290341415,-2.21766492551939));
#10716=CARTESIAN_POINT('Ctrl Pts',(2.82047457316189,55.2169382222468,-2.19965231451423));
#10717=CARTESIAN_POINT('Ctrl Pts',(2.8153526628751,55.2386030649626,-2.18220983334552));
#10718=CARTESIAN_POINT('Ctrl Pts',(2.81055920641232,55.2588786017284,-2.16588588985499));
#10719=CARTESIAN_POINT('Ctrl Pts',(2.80680052944647,55.2798164625832,-2.15006131614833));
#10720=CARTESIAN_POINT('Ctrl Pts',(2.8042702594812,55.3013208330089,-2.13495270927354));
#10721=CARTESIAN_POINT('Ctrl Pts',(2.80195466870913,55.3210006784011,-2.1211259828221));
#10722=CARTESIAN_POINT('Ctrl Pts',(2.80066799680603,55.3411552064162,-2.10789905750761));
#10723=CARTESIAN_POINT('Ctrl Pts',(2.8005704592906,55.3616930895013,-2.09546976536745));
#10724=CARTESIAN_POINT('',(2.79999999653565,55.7079964402821,-2.));
#10725=CARTESIAN_POINT('Ctrl Pts',(2.79999999999999,55.359994587709,-2.09491355855717));
#10726=CARTESIAN_POINT('Ctrl Pts',(2.79999999999999,55.3882860920536,-2.07799898836919));
#10727=CARTESIAN_POINT('Ctrl Pts',(2.80000000000001,55.4179318200166,-2.0632732682766));
#10728=CARTESIAN_POINT('Ctrl Pts',(2.80000000000001,55.530483252799,-2.01733304327692));
#10729=CARTESIAN_POINT('Ctrl Pts',(2.79999999999996,55.6192843749741,-2.));
#10730=CARTESIAN_POINT('Ctrl Pts',(2.79999999999996,55.7079964361128,-2.));
#10731=CARTESIAN_POINT('Ctrl Pts',(2.80000021990589,55.7079968150647,-1.99998051174467));
#10732=CARTESIAN_POINT('Ctrl Pts',(2.1959878240584,56.0680119999874,-1.99998070337318));
#10733=CARTESIAN_POINT('Ctrl Pts',(1.48287989181725,56.2388471215568,-1.99998078197634));
#10734=CARTESIAN_POINT('Ctrl Pts',(0.780890281868511,56.2437394329846,-1.9999807748488));
#10735=CARTESIAN_POINT('Ctrl Pts',(0.6,55.8,0.));
#10736=CARTESIAN_POINT('Ctrl Pts',(0.6,55.8,55.8));
#10737=CARTESIAN_POINT('Ctrl Pts',(0.600000000000001,0.,55.8));
#10738=CARTESIAN_POINT('Ctrl Pts',(0.600000000000001,-55.8,55.8));
#10739=CARTESIAN_POINT('Ctrl Pts',(0.600000000000001,-55.8,0.));
#10740=CARTESIAN_POINT('Ctrl Pts',(0.600000000000001,-55.8,-55.8));
#10741=CARTESIAN_POINT('Ctrl Pts',(0.600000000000001,0.,-55.8));
#10742=CARTESIAN_POINT('Ctrl Pts',(0.6,55.8,-55.8));
#10743=CARTESIAN_POINT('Ctrl Pts',(0.6,55.8,0.));
#10744=CARTESIAN_POINT('Ctrl Pts',(0.701236460530903,55.8018466247247,0.));
#10745=CARTESIAN_POINT('Ctrl Pts',(0.701236460530903,55.8018466247247,55.8018466247247));
#10746=CARTESIAN_POINT('Ctrl Pts',(0.701236460530903,0.,55.8018466247247));
#10747=CARTESIAN_POINT('Ctrl Pts',(0.701236460530903,-55.8018466247247,
55.8018466247247));
#10748=CARTESIAN_POINT('Ctrl Pts',(0.701236460530903,-55.8018466247247,
0.));
#10749=CARTESIAN_POINT('Ctrl Pts',(0.701236460530903,-55.8018466247247,
-55.8018466247247));
#10750=CARTESIAN_POINT('Ctrl Pts',(0.701236460530903,0.,-55.8018466247247));
#10751=CARTESIAN_POINT('Ctrl Pts',(0.701236460530903,55.8018466247247,-55.8018466247247));
#10752=CARTESIAN_POINT('Ctrl Pts',(0.701236460530903,55.8018466247247,0.));
#10753=CARTESIAN_POINT('Ctrl Pts',(0.900815345510183,55.8004649202247,0.));
#10754=CARTESIAN_POINT('Ctrl Pts',(0.900815345510183,55.8004649202247,55.8004649202247));
#10755=CARTESIAN_POINT('Ctrl Pts',(0.900815345510182,0.,55.8004649202247));
#10756=CARTESIAN_POINT('Ctrl Pts',(0.900815345510181,-55.8004649202247,
55.8004649202247));
#10757=CARTESIAN_POINT('Ctrl Pts',(0.900815345510181,-55.8004649202247,
0.));
#10758=CARTESIAN_POINT('Ctrl Pts',(0.900815345510181,-55.8004649202247,
-55.8004649202247));
#10759=CARTESIAN_POINT('Ctrl Pts',(0.900815345510182,0.,-55.8004649202247));
#10760=CARTESIAN_POINT('Ctrl Pts',(0.900815345510183,55.8004649202247,-55.8004649202247));
#10761=CARTESIAN_POINT('Ctrl Pts',(0.900815345510183,55.8004649202247,0.));
#10762=CARTESIAN_POINT('Ctrl Pts',(1.1915014799956,55.7831674035309,0.));
#10763=CARTESIAN_POINT('Ctrl Pts',(1.1915014799956,55.7831674035309,55.7831674035309));
#10764=CARTESIAN_POINT('Ctrl Pts',(1.1915014799956,0.,55.7831674035309));
#10765=CARTESIAN_POINT('Ctrl Pts',(1.1915014799956,-55.7831674035309,55.7831674035309));
#10766=CARTESIAN_POINT('Ctrl Pts',(1.1915014799956,-55.7831674035309,0.));
#10767=CARTESIAN_POINT('Ctrl Pts',(1.1915014799956,-55.7831674035309,-55.7831674035309));
#10768=CARTESIAN_POINT('Ctrl Pts',(1.1915014799956,0.,-55.7831674035309));
#10769=CARTESIAN_POINT('Ctrl Pts',(1.1915014799956,55.7831674035309,-55.7831674035309));
#10770=CARTESIAN_POINT('Ctrl Pts',(1.1915014799956,55.7831674035309,0.));
#10771=CARTESIAN_POINT('Ctrl Pts',(1.56159311954184,55.7294336445653,0.));
#10772=CARTESIAN_POINT('Ctrl Pts',(1.56159311954184,55.7294336445653,55.7294336445653));
#10773=CARTESIAN_POINT('Ctrl Pts',(1.56159311954184,0.,55.7294336445653));
#10774=CARTESIAN_POINT('Ctrl Pts',(1.56159311954184,-55.7294336445653,55.7294336445653));
#10775=CARTESIAN_POINT('Ctrl Pts',(1.56159311954184,-55.7294336445653,0.));
#10776=CARTESIAN_POINT('Ctrl Pts',(1.56159311954184,-55.7294336445653,-55.7294336445653));
#10777=CARTESIAN_POINT('Ctrl Pts',(1.56159311954184,0.,-55.7294336445653));
#10778=CARTESIAN_POINT('Ctrl Pts',(1.56159311954184,55.7294336445653,-55.7294336445653));
#10779=CARTESIAN_POINT('Ctrl Pts',(1.56159311954184,55.7294336445653,0.));
#10780=CARTESIAN_POINT('Ctrl Pts',(1.99433075254501,55.6097757263875,0.));
#10781=CARTESIAN_POINT('Ctrl Pts',(1.99433075254501,55.6097757263875,55.6097757263875));
#10782=CARTESIAN_POINT('Ctrl Pts',(1.99433075254501,0.,55.6097757263875));
#10783=CARTESIAN_POINT('Ctrl Pts',(1.99433075254501,-55.6097757263875,55.6097757263875));
#10784=CARTESIAN_POINT('Ctrl Pts',(1.99433075254501,-55.6097757263875,0.));
#10785=CARTESIAN_POINT('Ctrl Pts',(1.99433075254501,-55.6097757263875,-55.6097757263875));
#10786=CARTESIAN_POINT('Ctrl Pts',(1.99433075254501,0.,-55.6097757263875));
#10787=CARTESIAN_POINT('Ctrl Pts',(1.99433075254501,55.6097757263875,-55.6097757263875));
#10788=CARTESIAN_POINT('Ctrl Pts',(1.99433075254501,55.6097757263875,0.));
#10789=CARTESIAN_POINT('Ctrl Pts',(2.39636115062391,55.4358658864373,0.));
#10790=CARTESIAN_POINT('Ctrl Pts',(2.39636115062391,55.4358658864373,55.4358658864373));
#10791=CARTESIAN_POINT('Ctrl Pts',(2.39636115062391,0.,55.4358658864373));
#10792=CARTESIAN_POINT('Ctrl Pts',(2.39636115062391,-55.4358658864373,55.4358658864373));
#10793=CARTESIAN_POINT('Ctrl Pts',(2.39636115062391,-55.4358658864373,0.));
#10794=CARTESIAN_POINT('Ctrl Pts',(2.39636115062391,-55.4358658864373,-55.4358658864373));
#10795=CARTESIAN_POINT('Ctrl Pts',(2.39636115062391,0.,-55.4358658864373));
#10796=CARTESIAN_POINT('Ctrl Pts',(2.39636115062391,55.4358658864373,-55.4358658864373));
#10797=CARTESIAN_POINT('Ctrl Pts',(2.39636115062391,55.4358658864373,0.));
#10798=CARTESIAN_POINT('Ctrl Pts',(2.7670687050864,55.2060224359905,0.));
#10799=CARTESIAN_POINT('Ctrl Pts',(2.7670687050864,55.2060224359905,55.2060224359905));
#10800=CARTESIAN_POINT('Ctrl Pts',(2.7670687050864,0.,55.2060224359905));
#10801=CARTESIAN_POINT('Ctrl Pts',(2.7670687050864,-55.2060224359905,55.2060224359905));
#10802=CARTESIAN_POINT('Ctrl Pts',(2.7670687050864,-55.2060224359905,0.));
#10803=CARTESIAN_POINT('Ctrl Pts',(2.7670687050864,-55.2060224359905,-55.2060224359905));
#10804=CARTESIAN_POINT('Ctrl Pts',(2.7670687050864,0.,-55.2060224359905));
#10805=CARTESIAN_POINT('Ctrl Pts',(2.7670687050864,55.2060224359905,-55.2060224359905));
#10806=CARTESIAN_POINT('Ctrl Pts',(2.7670687050864,55.2060224359905,0.));
#10807=CARTESIAN_POINT('Ctrl Pts',(3.10660035178773,54.9194536393824,0.));
#10808=CARTESIAN_POINT('Ctrl Pts',(3.10660035178773,54.9194536393824,54.9194536393824));
#10809=CARTESIAN_POINT('Ctrl Pts',(3.10660035178772,0.,54.9194536393824));
#10810=CARTESIAN_POINT('Ctrl Pts',(3.10660035178772,-54.9194536393824,54.9194536393824));
#10811=CARTESIAN_POINT('Ctrl Pts',(3.10660035178772,-54.9194536393824,0.));
#10812=CARTESIAN_POINT('Ctrl Pts',(3.10660035178772,-54.9194536393824,-54.9194536393824));
#10813=CARTESIAN_POINT('Ctrl Pts',(3.10660035178772,0.,-54.9194536393824));
#10814=CARTESIAN_POINT('Ctrl Pts',(3.10660035178773,54.9194536393824,-54.9194536393824));
#10815=CARTESIAN_POINT('Ctrl Pts',(3.10660035178773,54.9194536393824,0.));
#10816=CARTESIAN_POINT('Ctrl Pts',(3.41599349838964,54.5765115223889,0.));
#10817=CARTESIAN_POINT('Ctrl Pts',(3.41599349838964,54.5765115223889,54.5765115223889));
#10818=CARTESIAN_POINT('Ctrl Pts',(3.41599349838964,0.,54.5765115223889));
#10819=CARTESIAN_POINT('Ctrl Pts',(3.41599349838964,-54.5765115223889,54.5765115223889));
#10820=CARTESIAN_POINT('Ctrl Pts',(3.41599349838964,-54.5765115223889,0.));
#10821=CARTESIAN_POINT('Ctrl Pts',(3.41599349838964,-54.5765115223889,-54.5765115223889));
#10822=CARTESIAN_POINT('Ctrl Pts',(3.41599349838964,0.,-54.5765115223889));
#10823=CARTESIAN_POINT('Ctrl Pts',(3.41599349838964,54.5765115223889,-54.5765115223889));
#10824=CARTESIAN_POINT('Ctrl Pts',(3.41599349838964,54.5765115223889,0.));
#10825=CARTESIAN_POINT('Ctrl Pts',(3.69673657250524,54.1781787924237,0.));
#10826=CARTESIAN_POINT('Ctrl Pts',(3.69673657250524,54.1781787924237,54.1781787924237));
#10827=CARTESIAN_POINT('Ctrl Pts',(3.69673657250524,0.,54.1781787924237));
#10828=CARTESIAN_POINT('Ctrl Pts',(3.69673657250524,-54.1781787924237,54.1781787924237));
#10829=CARTESIAN_POINT('Ctrl Pts',(3.69673657250524,-54.1781787924237,0.));
#10830=CARTESIAN_POINT('Ctrl Pts',(3.69673657250524,-54.1781787924237,-54.1781787924237));
#10831=CARTESIAN_POINT('Ctrl Pts',(3.69673657250524,0.,-54.1781787924237));
#10832=CARTESIAN_POINT('Ctrl Pts',(3.69673657250524,54.1781787924237,-54.1781787924237));
#10833=CARTESIAN_POINT('Ctrl Pts',(3.69673657250524,54.1781787924237,0.));
#10834=CARTESIAN_POINT('Ctrl Pts',(3.95058412182039,53.7259602136685,0.));
#10835=CARTESIAN_POINT('Ctrl Pts',(3.95058412182039,53.7259602136685,53.7259602136685));
#10836=CARTESIAN_POINT('Ctrl Pts',(3.95058412182039,0.,53.7259602136685));
#10837=CARTESIAN_POINT('Ctrl Pts',(3.95058412182039,-53.7259602136685,53.7259602136685));
#10838=CARTESIAN_POINT('Ctrl Pts',(3.95058412182039,-53.7259602136685,0.));
#10839=CARTESIAN_POINT('Ctrl Pts',(3.95058412182039,-53.7259602136685,-53.7259602136685));
#10840=CARTESIAN_POINT('Ctrl Pts',(3.95058412182039,0.,-53.7259602136685));
#10841=CARTESIAN_POINT('Ctrl Pts',(3.95058412182039,53.7259602136685,-53.7259602136685));
#10842=CARTESIAN_POINT('Ctrl Pts',(3.95058412182039,53.7259602136685,0.));
#10843=CARTESIAN_POINT('Ctrl Pts',(4.17937157605894,53.2217823983375,0.));
#10844=CARTESIAN_POINT('Ctrl Pts',(4.17937157605894,53.2217823983375,53.2217823983375));
#10845=CARTESIAN_POINT('Ctrl Pts',(4.17937157605894,0.,53.2217823983375));
#10846=CARTESIAN_POINT('Ctrl Pts',(4.17937157605894,-53.2217823983375,53.2217823983375));
#10847=CARTESIAN_POINT('Ctrl Pts',(4.17937157605894,-53.2217823983375,0.));
#10848=CARTESIAN_POINT('Ctrl Pts',(4.17937157605894,-53.2217823983375,-53.2217823983375));
#10849=CARTESIAN_POINT('Ctrl Pts',(4.17937157605894,0.,-53.2217823983375));
#10850=CARTESIAN_POINT('Ctrl Pts',(4.17937157605894,53.2217823983375,-53.2217823983375));
#10851=CARTESIAN_POINT('Ctrl Pts',(4.17937157605894,53.2217823983375,0.));
#10852=CARTESIAN_POINT('Ctrl Pts',(4.38495097171173,52.6681920799401,0.));
#10853=CARTESIAN_POINT('Ctrl Pts',(4.38495097171173,52.6681920799401,52.6681920799401));
#10854=CARTESIAN_POINT('Ctrl Pts',(4.38495097171173,0.,52.6681920799401));
#10855=CARTESIAN_POINT('Ctrl Pts',(4.38495097171173,-52.6681920799401,52.6681920799401));
#10856=CARTESIAN_POINT('Ctrl Pts',(4.38495097171173,-52.6681920799401,0.));
#10857=CARTESIAN_POINT('Ctrl Pts',(4.38495097171173,-52.6681920799401,-52.6681920799401));
#10858=CARTESIAN_POINT('Ctrl Pts',(4.38495097171173,0.,-52.6681920799401));
#10859=CARTESIAN_POINT('Ctrl Pts',(4.38495097171173,52.6681920799401,-52.6681920799401));
#10860=CARTESIAN_POINT('Ctrl Pts',(4.38495097171173,52.6681920799401,0.));
#10861=CARTESIAN_POINT('Ctrl Pts',(4.56903002475152,52.0679652261342,0.));
#10862=CARTESIAN_POINT('Ctrl Pts',(4.56903002475152,52.0679652261342,52.0679652261342));
#10863=CARTESIAN_POINT('Ctrl Pts',(4.56903002475152,0.,52.0679652261342));
#10864=CARTESIAN_POINT('Ctrl Pts',(4.56903002475152,-52.0679652261342,52.0679652261342));
#10865=CARTESIAN_POINT('Ctrl Pts',(4.56903002475152,-52.0679652261342,0.));
#10866=CARTESIAN_POINT('Ctrl Pts',(4.56903002475152,-52.0679652261342,-52.0679652261342));
#10867=CARTESIAN_POINT('Ctrl Pts',(4.56903002475152,0.,-52.0679652261342));
#10868=CARTESIAN_POINT('Ctrl Pts',(4.56903002475152,52.0679652261342,-52.0679652261342));
#10869=CARTESIAN_POINT('Ctrl Pts',(4.56903002475152,52.0679652261342,0.));
#10870=CARTESIAN_POINT('Ctrl Pts',(4.73302863242595,51.423645039376,0.));
#10871=CARTESIAN_POINT('Ctrl Pts',(4.73302863242595,51.423645039376,51.423645039376));
#10872=CARTESIAN_POINT('Ctrl Pts',(4.73302863242595,0.,51.423645039376));
#10873=CARTESIAN_POINT('Ctrl Pts',(4.73302863242595,-51.423645039376,51.423645039376));
#10874=CARTESIAN_POINT('Ctrl Pts',(4.73302863242595,-51.423645039376,0.));
#10875=CARTESIAN_POINT('Ctrl Pts',(4.73302863242595,-51.423645039376,-51.423645039376));
#10876=CARTESIAN_POINT('Ctrl Pts',(4.73302863242595,0.,-51.423645039376));
#10877=CARTESIAN_POINT('Ctrl Pts',(4.73302863242595,51.423645039376,-51.423645039376));
#10878=CARTESIAN_POINT('Ctrl Pts',(4.73302863242595,51.423645039376,0.));
#10879=CARTESIAN_POINT('Ctrl Pts',(4.84900124161322,50.8745342238058,0.));
#10880=CARTESIAN_POINT('Ctrl Pts',(4.84900124161322,50.8745342238058,50.8745342238058));
#10881=CARTESIAN_POINT('Ctrl Pts',(4.84900124161322,0.,50.8745342238058));
#10882=CARTESIAN_POINT('Ctrl Pts',(4.84900124161322,-50.8745342238058,50.8745342238058));
#10883=CARTESIAN_POINT('Ctrl Pts',(4.84900124161322,-50.8745342238058,0.));
#10884=CARTESIAN_POINT('Ctrl Pts',(4.84900124161322,-50.8745342238058,-50.8745342238058));
#10885=CARTESIAN_POINT('Ctrl Pts',(4.84900124161322,0.,-50.8745342238058));
#10886=CARTESIAN_POINT('Ctrl Pts',(4.84900124161322,50.8745342238058,-50.8745342238058));
#10887=CARTESIAN_POINT('Ctrl Pts',(4.84900124161322,50.8745342238058,0.));
#10888=CARTESIAN_POINT('Ctrl Pts',(4.92769824210582,50.4443513809858,0.));
#10889=CARTESIAN_POINT('Ctrl Pts',(4.92769824210582,50.4443513809858,50.4443513809858));
#10890=CARTESIAN_POINT('Ctrl Pts',(4.92769824210582,0.,50.4443513809858));
#10891=CARTESIAN_POINT('Ctrl Pts',(4.92769824210582,-50.4443513809858,50.4443513809858));
#10892=CARTESIAN_POINT('Ctrl Pts',(4.92769824210582,-50.4443513809858,0.));
#10893=CARTESIAN_POINT('Ctrl Pts',(4.92769824210582,-50.4443513809858,-50.4443513809858));
#10894=CARTESIAN_POINT('Ctrl Pts',(4.92769824210582,0.,-50.4443513809858));
#10895=CARTESIAN_POINT('Ctrl Pts',(4.92769824210582,50.4443513809858,-50.4443513809858));
#10896=CARTESIAN_POINT('Ctrl Pts',(4.92769824210582,50.4443513809858,0.));
#10897=CARTESIAN_POINT('Ctrl Pts',(4.97650848841056,50.1494665212081,0.));
#10898=CARTESIAN_POINT('Ctrl Pts',(4.97650848841056,50.1494665212081,50.1494665212081));
#10899=CARTESIAN_POINT('Ctrl Pts',(4.97650848841056,0.,50.1494665212081));
#10900=CARTESIAN_POINT('Ctrl Pts',(4.97650848841056,-50.1494665212081,50.1494665212081));
#10901=CARTESIAN_POINT('Ctrl Pts',(4.97650848841056,-50.1494665212081,0.));
#10902=CARTESIAN_POINT('Ctrl Pts',(4.97650848841056,-50.1494665212081,-50.1494665212081));
#10903=CARTESIAN_POINT('Ctrl Pts',(4.97650848841056,0.,-50.1494665212081));
#10904=CARTESIAN_POINT('Ctrl Pts',(4.97650848841056,50.1494665212081,-50.1494665212081));
#10905=CARTESIAN_POINT('Ctrl Pts',(4.97650848841056,50.1494665212081,0.));
#10906=CARTESIAN_POINT('Ctrl Pts',(5.,50.,0.));
#10907=CARTESIAN_POINT('Ctrl Pts',(5.,50.,50.));
#10908=CARTESIAN_POINT('Ctrl Pts',(5.,0.,50.));
#10909=CARTESIAN_POINT('Ctrl Pts',(5.,-50.,50.));
#10910=CARTESIAN_POINT('Ctrl Pts',(5.,-50.,0.));
#10911=CARTESIAN_POINT('Ctrl Pts',(5.,-50.,-50.));
#10912=CARTESIAN_POINT('Ctrl Pts',(5.,0.,-50.));
#10913=CARTESIAN_POINT('Ctrl Pts',(5.,50.,-50.));
#10914=CARTESIAN_POINT('Ctrl Pts',(5.,50.,0.));
#10915=CARTESIAN_POINT('',(2.97156409628618,54.9665637470307,2.48298719598219));
#10916=CARTESIAN_POINT('Ctrl Pts',(2.97156409628618,54.9665637470307,2.48298719598219));
#10917=CARTESIAN_POINT('Ctrl Pts',(2.38240222522867,55.4903197198984,2.47922620961122));
#10918=CARTESIAN_POINT('Ctrl Pts',(1.59934858958684,55.7362874995129,2.47769305658212));
#10919=CARTESIAN_POINT('Ctrl Pts',(0.772591931467188,55.7451294709179,2.47780062126727));
#10920=CARTESIAN_POINT('',(2.97156409628601,55.0226167641255,6.66133814775094E-15));
#10921=CARTESIAN_POINT('Ctrl Pts',(2.971564096286,55.0226075943045,1.82631687550838E-14));
#10922=CARTESIAN_POINT('Ctrl Pts',(2.971564096286,55.0226075940038,0.827947557198553));
#10923=CARTESIAN_POINT('Ctrl Pts',(2.97156409628599,55.0039260136328,1.65588852538752));
#10924=CARTESIAN_POINT('Ctrl Pts',(2.97156409628599,54.9665637470306,2.48298719598933));
#10925=CARTESIAN_POINT('',(4.99841192763649,50.010089934565,-1.0547118733939E-14));
#10926=CARTESIAN_POINT('Ctrl Pts',(4.99841192763651,50.0100899345649,0.));
#10927=CARTESIAN_POINT('Ctrl Pts',(4.97518900611397,50.157429856102,0.));
#10928=CARTESIAN_POINT('Ctrl Pts',(4.92663484069112,50.450160402527,0.));
#10929=CARTESIAN_POINT('Ctrl Pts',(4.84821789314001,50.8782420415372,0.));
#10930=CARTESIAN_POINT('Ctrl Pts',(4.73258563268563,51.4253855033925,0.));
#10931=CARTESIAN_POINT('Ctrl Pts',(4.56903002475152,52.0679652261342,0.));
#10932=CARTESIAN_POINT('Ctrl Pts',(4.38495097171173,52.6681920799401,0.));
#10933=CARTESIAN_POINT('Ctrl Pts',(4.17937157605894,53.2217823983375,0.));
#10934=CARTESIAN_POINT('Ctrl Pts',(3.95058412182039,53.7259602136685,0.));
#10935=CARTESIAN_POINT('Ctrl Pts',(3.69673657250524,54.1781787924237,0.));
#10936=CARTESIAN_POINT('Ctrl Pts',(3.45047359613994,54.527589384204,0.));
#10937=CARTESIAN_POINT('Ctrl Pts',(3.24393642390649,54.765582391618,0.));
#10938=CARTESIAN_POINT('Ctrl Pts',(3.08990662218085,54.9172980064984,0.));
#10939=CARTESIAN_POINT('Ctrl Pts',(2.99751746911325,55.0000067011129,0.));
#10940=CARTESIAN_POINT('Ctrl Pts',(2.97156409628601,55.0226167641255,0.));
#10941=CARTESIAN_POINT('Ctrl Pts',(4.99841192763649,50.0100899345651,-2.44355213456396E-14));
#10942=CARTESIAN_POINT('Ctrl Pts',(4.99841192763649,50.010089934565,-7.48115762363152));
#10943=CARTESIAN_POINT('Ctrl Pts',(4.9984119276365,46.6017252207067,-22.4413792780267));
#10944=CARTESIAN_POINT('Ctrl Pts',(4.99841192763649,33.8387987663498,-38.4316981785149));
#10945=CARTESIAN_POINT('Ctrl Pts',(4.9984119276365,18.5446192921948,-47.2509187816055));
#10946=CARTESIAN_POINT('Ctrl Pts',(4.99841192763649,6.25354094871083,-50.0596743547279));
#10947=CARTESIAN_POINT('Ctrl Pts',(4.99841192763649,-3.75050037564627,-50.055717263026));
#10948=CARTESIAN_POINT('Ctrl Pts',(4.99841192763649,-13.6423328766374,-48.5678652060244));
#10949=CARTESIAN_POINT('Ctrl Pts',(4.9984119276365,-25.3805953459256,-43.9618581545187));
#10950=CARTESIAN_POINT('Ctrl Pts',(4.99841192763649,-37.210931604044,-34.5275648165732));
#10951=CARTESIAN_POINT('Ctrl Pts',(4.99841192763649,-45.7357692537155,-22.0258961118735));
#10952=CARTESIAN_POINT('Ctrl Pts',(4.9984119276365,-50.1946948077045,-7.566025938944));
#10953=CARTESIAN_POINT('Ctrl Pts',(4.9984119276365,-50.1960569239472,7.56522373629383));
#10954=CARTESIAN_POINT('Ctrl Pts',(4.99841192763649,-45.7352070158957,22.0246092149029));
#10955=CARTESIAN_POINT('Ctrl Pts',(4.99841192763649,-37.2116055718427,34.5267335901821));
#10956=CARTESIAN_POINT('Ctrl Pts',(4.99841192763649,-25.3814385247641,43.9614029395442));
#10957=CARTESIAN_POINT('Ctrl Pts',(4.99841192763649,-11.2963143151676,49.4899240087747));
#10958=CARTESIAN_POINT('Ctrl Pts',(4.99841192763649,3.7937298863526,50.6205829747067));
#10959=CARTESIAN_POINT('Ctrl Pts',(4.99841192763649,18.5440439702159,47.2521255691362));
#10960=CARTESIAN_POINT('Ctrl Pts',(4.99841192763649,33.8380966958625,38.4319339724568));
#10961=CARTESIAN_POINT('Ctrl Pts',(4.9984119276365,46.6012579438089,22.4429169923092));
#10962=CARTESIAN_POINT('Ctrl Pts',(4.99841192763649,50.010089934565,7.48115762363149));
#10963=CARTESIAN_POINT('Ctrl Pts',(4.99841192763649,50.010089934565,-2.22455486416984E-15));
#10964=CARTESIAN_POINT('Ctrl Pts',(2.971564096286,54.9665637470309,-2.48298719598223));
#10965=CARTESIAN_POINT('Ctrl Pts',(2.971564096286,55.0039266101128,-1.65587532094447));
#10966=CARTESIAN_POINT('Ctrl Pts',(2.971564096286,55.0226075946053,-0.827934366072422));
#10967=CARTESIAN_POINT('Ctrl Pts',(2.971564096286,55.0226075943045,1.82631687550838E-14));
#10968=CARTESIAN_POINT('Ctrl Pts',(0.780904059217545,56.2445672509427,2.));
#10969=CARTESIAN_POINT('Ctrl Pts',(1.68852632773542,56.2382423732899,2.));
#10970=CARTESIAN_POINT('Ctrl Pts',(2.61486131739033,55.9545502327436,2.));
#10971=CARTESIAN_POINT('Ctrl Pts',(3.30000000000027,55.3431808226539,2.));
#10972=CARTESIAN_POINT('Ctrl Pts',(0.776592785321951,55.9855224999279,1.99373831640894));
#10973=CARTESIAN_POINT('Ctrl Pts',(1.64227856307928,55.977965882459,1.99374127522468));
#10974=CARTESIAN_POINT('Ctrl Pts',(2.49433299618752,55.7131454773729,1.99369822532176));
#10975=CARTESIAN_POINT('Ctrl Pts',(3.12847993397336,55.1464989588648,1.99359023604657));
#10976=CARTESIAN_POINT('Ctrl Pts',(0.772679250843364,55.750376093287,2.21869746782962));
#10977=CARTESIAN_POINT('Ctrl Pts',(1.60029571178559,55.741676045719,2.21863137550334));
#10978=CARTESIAN_POINT('Ctrl Pts',(2.38490822912943,55.4942251910797,2.21958486623663));
#10979=CARTESIAN_POINT('Ctrl Pts',(2.97318977758978,54.9684279139246,2.22195490734826));
#10980=CARTESIAN_POINT('Ctrl Pts',(0.772591931467188,55.7451294709179,2.47780062126727));
#10981=CARTESIAN_POINT('Ctrl Pts',(1.59934858958684,55.7362874995129,2.47769305658212));
#10982=CARTESIAN_POINT('Ctrl Pts',(2.38240222522867,55.4903197198984,2.47922620961122));
#10983=CARTESIAN_POINT('Ctrl Pts',(2.97156409628618,54.9665637470307,2.48298719598219));
#10984=CARTESIAN_POINT('',(2.79999999922762,55.7079964370423,2.));
#10985=CARTESIAN_POINT('Ctrl Pts',(0.780904059217545,56.2445672509427,2.));
#10986=CARTESIAN_POINT('Ctrl Pts',(1.4829815941067,56.2396747371019,2.));
#10987=CARTESIAN_POINT('Ctrl Pts',(2.19625600357399,56.0688177741594,2.));
#10988=CARTESIAN_POINT('Ctrl Pts',(2.80042852309129,55.7087104005398,2.));
#10989=CARTESIAN_POINT('',(2.8,55.359994587709,2.09491355855719));
#10990=CARTESIAN_POINT('Ctrl Pts',(2.79999999999999,55.7079964361128,2.));
#10991=CARTESIAN_POINT('Ctrl Pts',(2.79999999999999,55.659531184896,2.));
#10992=CARTESIAN_POINT('Ctrl Pts',(2.79999999998947,55.6110538105124,2.00517381305814));
#10993=CARTESIAN_POINT('Ctrl Pts',(2.79999999998947,55.5164155335608,2.02544396016552));
#10994=CARTESIAN_POINT('Ctrl Pts',(2.79999999999996,55.4701792356063,2.04052661685823));
#10995=CARTESIAN_POINT('Ctrl Pts',(2.79999999999996,55.4034746461591,2.07062671510575));
#10996=CARTESIAN_POINT('Ctrl Pts',(2.79999999999998,55.3813520773532,2.08214461021052));
#10997=CARTESIAN_POINT('Ctrl Pts',(2.79999999999998,55.359994587709,2.0949135585572));
#10998=CARTESIAN_POINT('Ctrl Pts',(2.97156409628599,54.9665637470306,2.48298719598933));
#10999=CARTESIAN_POINT('Ctrl Pts',(2.97106588998616,54.9670303350916,2.48227619063589));
#11000=CARTESIAN_POINT('Ctrl Pts',(2.97056853930023,54.9674978995121,2.48156522401649));
#11001=CARTESIAN_POINT('Ctrl Pts',(2.91166555208744,55.0230844632908,2.39722260558573));
#11002=CARTESIAN_POINT('Ctrl Pts',(2.8635616296325,55.0931658791427,2.31195530150665));
#11003=CARTESIAN_POINT('Ctrl Pts',(2.81284170698683,55.2301922759081,2.18416468374735));
#11004=CARTESIAN_POINT('Ctrl Pts',(2.8,55.2927619192075,2.13510978412522));
#11005=CARTESIAN_POINT('Ctrl Pts',(2.8,55.359994587709,2.09491355855718));
#11006=CARTESIAN_POINT('Origin',(1.15,56.75,2.));
#11007=CARTESIAN_POINT('',(2.80000000000027,57.2719725101481,2.));
#11008=CARTESIAN_POINT('Ctrl Pts',(2.80000000335065,57.271971836207,1.999973299767));
#11009=CARTESIAN_POINT('Ctrl Pts',(2.0202116745349,57.268095273033,1.99997329939139));
#11010=CARTESIAN_POINT('Ctrl Pts',(1.2401748212868,57.1446587362222,1.99997332725321));
#11011=CARTESIAN_POINT('Ctrl Pts',(0.499674955335824,56.8988024033561,1.99997341417823));
#11012=CARTESIAN_POINT('',(2.8,55.,2.));
#11013=CARTESIAN_POINT('Ctrl Pts',(5.00202436963841,49.989878151808,-2.22044604925031E-15));
#11014=CARTESIAN_POINT('Ctrl Pts',(5.00202436963841,49.989878151808,7.4781340831248));
#11015=CARTESIAN_POINT('Ctrl Pts',(5.00202436963841,46.5824238544682,22.4338465954497));
#11016=CARTESIAN_POINT('Ctrl Pts',(5.00202436963841,33.8244208904356,38.4164015488718));
#11017=CARTESIAN_POINT('Ctrl Pts',(5.00202436963841,18.5365493188635,47.2330284289778));
#11018=CARTESIAN_POINT('Ctrl Pts',(5.0020243696384,3.7921966348747,50.6001244586861));
#11019=CARTESIAN_POINT('Ctrl Pts',(5.0020243696384,-11.291748863452,49.4699224532078));
#11020=CARTESIAN_POINT('Ctrl Pts',(5.0020243696384,-25.3711805123871,43.9436357584199));
#11021=CARTESIAN_POINT('Ctrl Pts',(5.0020243696384,-37.1965663489811,34.5127794693327));
#11022=CARTESIAN_POINT('Ctrl Pts',(5.0020243696384,-45.716722944586,22.0157078788456));
#11023=CARTESIAN_POINT('Ctrl Pts',(5.00202436963841,-50.1757699818694,7.56216622012327));
#11024=CARTESIAN_POINT('Ctrl Pts',(5.00202436963842,-50.1744084161316,-7.56296809855995));
#11025=CARTESIAN_POINT('Ctrl Pts',(5.00202436963841,-45.7172849551752,-22.0169942557115));
#11026=CARTESIAN_POINT('Ctrl Pts',(5.00202436963841,-37.1958926535692,-34.5136103597803));
#11027=CARTESIAN_POINT('Ctrl Pts',(5.00202436963841,-25.3703376743228,-43.9440907894173));
#11028=CARTESIAN_POINT('Ctrl Pts',(5.0020243696384,-13.6368192719076,-48.5482363043008));
#11029=CARTESIAN_POINT('Ctrl Pts',(5.0020243696384,-3.74898459555225,-50.0354870397972));
#11030=CARTESIAN_POINT('Ctrl Pts',(5.0020243696384,6.25101355451332,-50.0394425322242));
#11031=CARTESIAN_POINT('Ctrl Pts',(5.00202436963841,18.5371244083236,-47.2318221291753));
#11032=CARTESIAN_POINT('Ctrl Pts',(5.0020243696384,33.8251226771782,-38.416165850227));
#11033=CARTESIAN_POINT('Ctrl Pts',(5.00202436963841,46.5828909425141,-22.4323095026409));
#11034=CARTESIAN_POINT('Ctrl Pts',(5.0020243696384,49.989878151808,-7.47813408312484));
#11035=CARTESIAN_POINT('Ctrl Pts',(5.0020243696384,49.989878151808,-2.44249065417534E-14));
#11036=CARTESIAN_POINT('Ctrl Pts',(5.00068205190813,49.9965897404593,-2.22119182093928E-15));
#11037=CARTESIAN_POINT('Ctrl Pts',(5.00068205190813,49.9965897404593,7.47913808945617));
#11038=CARTESIAN_POINT('Ctrl Pts',(5.00068205190813,46.588677961852,22.4368585402377));
#11039=CARTESIAN_POINT('Ctrl Pts',(5.00068205190813,33.8289621217263,38.42155929466));
#11040=CARTESIAN_POINT('Ctrl Pts',(5.00068205190813,18.5390380165073,47.2393698858715));
#11041=CARTESIAN_POINT('Ctrl Pts',(5.00068205190813,3.79270577122635,50.6069179783561));
#11042=CARTESIAN_POINT('Ctrl Pts',(5.00068205190813,-11.2932648818068,49.4765642331324));
#11043=CARTESIAN_POINT('Ctrl Pts',(5.00068205190813,-25.3745868205016,43.9495355848871));
#11044=CARTESIAN_POINT('Ctrl Pts',(5.00068205190813,-37.2015603209659,34.5174131189366));
#11045=CARTESIAN_POINT('Ctrl Pts',(5.00068205190813,-45.7228608238853,22.0186636847214));
#11046=CARTESIAN_POINT('Ctrl Pts',(5.00068205190814,-50.1825065281432,7.5631815085935));
#11047=CARTESIAN_POINT('Ctrl Pts',(5.00068205190814,-50.1811447796148,-7.5639834947219));
#11048=CARTESIAN_POINT('Ctrl Pts',(5.00068205190813,-45.7234229099287,-22.019950234269));
#11049=CARTESIAN_POINT('Ctrl Pts',(5.00068205190813,-37.2008865351074,-34.5182441209412));
#11050=CARTESIAN_POINT('Ctrl Pts',(5.00068205190814,-25.3737438692996,-43.9499906769628));
#11051=CARTESIAN_POINT('Ctrl Pts',(5.00068205190813,-13.6386501369243,-48.5547543396211));
#11052=CARTESIAN_POINT('Ctrl Pts',(5.00068205190813,-3.74948793029787,-50.0422047518384));
#11053=CARTESIAN_POINT('Ctrl Pts',(5.00068205190813,6.25185280903391,-50.0461607753142));
#11054=CARTESIAN_POINT('Ctrl Pts',(5.00068205190813,18.5396131832233,-47.2381634241137));
#11055=CARTESIAN_POINT('Ctrl Pts',(5.00068205190814,33.8296640026347,-38.4213235643879));
#11056=CARTESIAN_POINT('Ctrl Pts',(5.00068205190814,46.5891451126407,-22.4353212410508));
#11057=CARTESIAN_POINT('Ctrl Pts',(5.00068205190813,49.9965897404593,-7.47913808945619));
#11058=CARTESIAN_POINT('Ctrl Pts',(5.00068205190813,49.9965897404594,-2.4429070022793E-14));
#11059=CARTESIAN_POINT('Ctrl Pts',(4.99947756609878,50.003328895164,-2.22256181089655E-15));
#11060=CARTESIAN_POINT('Ctrl Pts',(4.99947756609878,50.003328895164,7.48014621959278));
#11061=CARTESIAN_POINT('Ctrl Pts',(4.99947756609879,46.5949577563329,22.4398828557256));
#11062=CARTESIAN_POINT('Ctrl Pts',(4.99947756609878,33.8335220049191,38.4267382245323));
#11063=CARTESIAN_POINT('Ctrl Pts',(4.99947756609878,18.5415369358535,47.2457373886046));
#11064=CARTESIAN_POINT('Ctrl Pts',(4.99947756609878,3.79321699871334,50.6137394006006));
#11065=CARTESIAN_POINT('Ctrl Pts',(4.99947756609877,-11.2947871268155,49.4832332924101));
#11066=CARTESIAN_POINT('Ctrl Pts',(4.99947756609878,-25.3780071191065,43.9554596433293));
#11067=CARTESIAN_POINT('Ctrl Pts',(4.99947756609878,-37.206574804386,34.5220658000138));
#11068=CARTESIAN_POINT('Ctrl Pts',(4.99947756609877,-45.729023912893,22.0216316307696));
#11069=CARTESIAN_POINT('Ctrl Pts',(4.99947756609878,-50.1892707429977,7.56420096713228));
#11070=CARTESIAN_POINT('Ctrl Pts',(4.99947756609879,-50.1879088109157,-7.56500306136105));
#11071=CARTESIAN_POINT('Ctrl Pts',(4.99947756609878,-45.7295860747013,-22.0229183537352));
#11072=CARTESIAN_POINT('Ctrl Pts',(4.99947756609878,-37.2059009277063,-34.522896914031));
#11073=CARTESIAN_POINT('Ctrl Pts',(4.99947756609878,-25.3771640542804,-43.9559147967486));
#11074=CARTESIAN_POINT('Ctrl Pts',(4.99947756609877,-13.6404885217781,-48.561299146034));
#11075=CARTESIAN_POINT('Ctrl Pts',(4.99947756609878,-3.74999333235333,-50.0489500550953));
#11076=CARTESIAN_POINT('Ctrl Pts',(4.99947756609877,6.25269551057625,-50.0529066118129));
#11077=CARTESIAN_POINT('Ctrl Pts',(4.99947756609878,18.5421121800959,-47.2445307642251));
#11078=CARTESIAN_POINT('Ctrl Pts',(4.99947756609877,33.8342239804377,-38.426502462485));
#11079=CARTESIAN_POINT('Ctrl Pts',(4.99947756609879,46.5954249700887,-22.438345349323));
#11080=CARTESIAN_POINT('Ctrl Pts',(4.99947756609877,50.003328895164,-7.48014621959283));
#11081=CARTESIAN_POINT('Ctrl Pts',(4.99947756609877,50.003328895164,-2.44326092853315E-14));
#11082=CARTESIAN_POINT('Ctrl Pts',(4.99841192763649,50.010089934565,-2.22455486416984E-15));
#11083=CARTESIAN_POINT('Ctrl Pts',(4.99841192763649,50.010089934565,7.48115762363149));
#11084=CARTESIAN_POINT('Ctrl Pts',(4.9984119276365,46.6012579438089,22.4429169923092));
#11085=CARTESIAN_POINT('Ctrl Pts',(4.99841192763649,33.8380966958625,38.4319339724568));
#11086=CARTESIAN_POINT('Ctrl Pts',(4.99841192763649,18.5440439702159,47.2521255691362));
#11087=CARTESIAN_POINT('Ctrl Pts',(4.99841192763649,3.7937298863526,50.6205829747067));
#11088=CARTESIAN_POINT('Ctrl Pts',(4.99841192763649,-11.2963143151676,49.4899240087747));
#11089=CARTESIAN_POINT('Ctrl Pts',(4.99841192763649,-25.3814385247641,43.9614029395442));
#11090=CARTESIAN_POINT('Ctrl Pts',(4.99841192763649,-37.2116055718427,34.5267335901821));
#11091=CARTESIAN_POINT('Ctrl Pts',(4.99841192763649,-45.7352070158957,22.0246092149029));
#11092=CARTESIAN_POINT('Ctrl Pts',(4.9984119276365,-50.1960569239472,7.56522373629383));
#11093=CARTESIAN_POINT('Ctrl Pts',(4.9984119276365,-50.1946948077045,-7.566025938944));
#11094=CARTESIAN_POINT('Ctrl Pts',(4.99841192763649,-45.7357692537155,-22.0258961118735));
#11095=CARTESIAN_POINT('Ctrl Pts',(4.99841192763649,-37.210931604044,-34.5275648165732));
#11096=CARTESIAN_POINT('Ctrl Pts',(4.9984119276365,-25.3805953459256,-43.9618581545187));
#11097=CARTESIAN_POINT('Ctrl Pts',(4.99841192763649,-13.6423328766374,-48.5678652060244));
#11098=CARTESIAN_POINT('Ctrl Pts',(4.99841192763649,-3.75050037564627,-50.055717263026));
#11099=CARTESIAN_POINT('Ctrl Pts',(4.99841192763649,6.25354094871083,-50.0596743547279));
#11100=CARTESIAN_POINT('Ctrl Pts',(4.9984119276365,18.5446192921948,-47.2509187816055));
#11101=CARTESIAN_POINT('Ctrl Pts',(4.99841192763649,33.8387987663498,-38.4316981785149));
#11102=CARTESIAN_POINT('Ctrl Pts',(4.9984119276365,46.6017252207067,-22.4413792780267));
#11103=CARTESIAN_POINT('Ctrl Pts',(4.99841192763649,50.010089934565,-7.48115762363152));
#11104=CARTESIAN_POINT('Ctrl Pts',(4.99841192763649,50.0100899345651,-2.44355213456396E-14));
#11105=CARTESIAN_POINT('',(5.00202436963841,49.989878151808,-2.22044604925031E-15));
#11106=CARTESIAN_POINT('Origin',(5.49231470748387,50.0879362193771,-4.44089209850063E-15));
#11107=CARTESIAN_POINT('',(5.00202436963841,-49.9893356667678,9.68104724163865E-7));
#11108=CARTESIAN_POINT('Ctrl Pts',(5.00202436963841,49.989878151808,-2.22044604925031E-15));
#11109=CARTESIAN_POINT('Ctrl Pts',(5.00202436963841,49.989878151808,7.4781340831248));
#11110=CARTESIAN_POINT('Ctrl Pts',(5.00202436963841,46.5824238544682,22.4338465954497));
#11111=CARTESIAN_POINT('Ctrl Pts',(5.00202436963841,33.8244208904356,38.4164015488718));
#11112=CARTESIAN_POINT('Ctrl Pts',(5.00202436963841,18.5365493188635,47.2330284289778));
#11113=CARTESIAN_POINT('Ctrl Pts',(5.0020243696384,3.7921966348747,50.6001244586861));
#11114=CARTESIAN_POINT('Ctrl Pts',(5.0020243696384,-11.291748863452,49.4699224532078));
#11115=CARTESIAN_POINT('Ctrl Pts',(5.0020243696384,-25.3711805123871,43.9436357584199));
#11116=CARTESIAN_POINT('Ctrl Pts',(5.0020243696384,-37.1965663489811,34.5127794693327));
#11117=CARTESIAN_POINT('Ctrl Pts',(5.0020243696384,-45.716722944586,22.0157078788456));
#11118=CARTESIAN_POINT('Ctrl Pts',(5.00202436963841,-49.4325545339432,9.9712225382536));
#11119=CARTESIAN_POINT('Ctrl Pts',(5.00202436963841,-49.9894453154963,2.49274641922705));
#11120=CARTESIAN_POINT('Ctrl Pts',(5.00202436963841,-49.9893356667678,9.68104723747532E-7));
#11121=CARTESIAN_POINT('Ctrl Pts',(5.00202436963841,-49.9893356667678,9.68104723747532E-7));
#11122=CARTESIAN_POINT('Ctrl Pts',(5.00202436963841,-49.9892260059575,-2.49301915037777));
#11123=CARTESIAN_POINT('Ctrl Pts',(5.00202436963841,-49.4315954300228,-9.9718397452934));
#11124=CARTESIAN_POINT('Ctrl Pts',(5.00202436963841,-45.7172849551752,-22.0169942557115));
#11125=CARTESIAN_POINT('Ctrl Pts',(5.00202436963841,-37.1958926535692,-34.5136103597803));
#11126=CARTESIAN_POINT('Ctrl Pts',(5.00202436963841,-25.3703376743228,-43.9440907894173));
#11127=CARTESIAN_POINT('Ctrl Pts',(5.0020243696384,-13.6368192719076,-48.5482363043008));
#11128=CARTESIAN_POINT('Ctrl Pts',(5.0020243696384,-3.74898459555225,-50.0354870397972));
#11129=CARTESIAN_POINT('Ctrl Pts',(5.0020243696384,6.25101355451332,-50.0394425322242));
#11130=CARTESIAN_POINT('Ctrl Pts',(5.00202436963841,18.5371244083236,-47.2318221291753));
#11131=CARTESIAN_POINT('Ctrl Pts',(5.0020243696384,33.8251226771782,-38.416165850227));
#11132=CARTESIAN_POINT('Ctrl Pts',(5.00202436963841,46.5828909425141,-22.4323095026409));
#11133=CARTESIAN_POINT('Ctrl Pts',(5.0020243696384,49.989878151808,-7.47813408312484));
#11134=CARTESIAN_POINT('Ctrl Pts',(5.0020243696384,49.989878151808,-2.44249065417534E-14));
#11135=CARTESIAN_POINT('Origin',(8.,0.,0.));
#11136=CARTESIAN_POINT('',(11.,-20.,-2.44929359829471E-15));
#11137=CARTESIAN_POINT('Origin',(11.,0.,0.));
#11138=CARTESIAN_POINT('',(8.,-35.,-4.28626379701574E-15));
#11139=CARTESIAN_POINT('Origin',(5.5,0.,0.));
#11140=CARTESIAN_POINT('',(5.5,-1.46957615897682E-15,12.));
#11141=CARTESIAN_POINT('',(5.5,-12.,-1.46957615897682E-15));
#11142=CARTESIAN_POINT('Origin',(5.5,0.,0.));
#11143=CARTESIAN_POINT('Origin',(5.5,0.,0.));
#11144=CARTESIAN_POINT('',(5.,-1.40834381901946E-15,11.5));
#11145=CARTESIAN_POINT('Origin',(5.5,-1.40834381901946E-15,11.5));
#11146=CARTESIAN_POINT('Origin',(5.,0.,0.));
#11147=CARTESIAN_POINT('Origin',(5.,12.,0.));
#11148=CARTESIAN_POINT('',(5.,7.8995253021938,3.));
#11149=CARTESIAN_POINT('',(5.,10.74,3.));
#11150=CARTESIAN_POINT('',(5.,10.31,3.));
#11151=CARTESIAN_POINT('',(5.,7.8995253021938,-3.));
#11152=CARTESIAN_POINT('Origin',(5.,0.,0.));
#11153=CARTESIAN_POINT('',(5.,10.74,-3.));
#11154=CARTESIAN_POINT('',(5.,10.31,-3.));
#11155=CARTESIAN_POINT('',(5.,10.74,0.));
#11156=CARTESIAN_POINT('Origin',(8.,0.,0.));
#11157=CARTESIAN_POINT('',(11.,-12.,-1.46957615897682E-15));
#11158=CARTESIAN_POINT('Origin',(11.,0.,0.));
#11159=CARTESIAN_POINT('',(8.,-12.,-1.46957615897682E-15));
#11160=CARTESIAN_POINT('Origin',(5.5,10.74,0.));
#11161=CARTESIAN_POINT('',(5.5,10.24,-2.5));
#11162=CARTESIAN_POINT('Origin',(5.5,10.74,-3.));
#11163=CARTESIAN_POINT('',(5.5,10.24,2.5));
#11164=CARTESIAN_POINT('',(5.5,10.24,0.));
#11165=CARTESIAN_POINT('Origin',(5.5,10.74,3.));
#11166=CARTESIAN_POINT('Origin',(5.5,10.31,3.));
#11167=CARTESIAN_POINT('',(5.5,7.8995253021938,2.5));
#11168=CARTESIAN_POINT('',(5.5,10.31,2.5));
#11169=CARTESIAN_POINT('Origin',(5.5,7.8995253021938,3.));
#11170=CARTESIAN_POINT('Origin',(5.5,7.8995253021938,3.));
#11171=CARTESIAN_POINT('',(5.5,7.43209776951961,2.82248520710059));
#11172=CARTESIAN_POINT('Origin',(5.5,7.8995253021938,3.));
#11173=CARTESIAN_POINT('Origin',(5.5,7.8995253021938,3.));
#11174=CARTESIAN_POINT('Origin',(5.5,0.,0.));
#11175=CARTESIAN_POINT('',(5.5,7.43209776951961,-2.82248520710059));
#11176=CARTESIAN_POINT('Origin',(5.5,0.,0.));
#11177=CARTESIAN_POINT('Origin',(5.5,7.8995253021938,-3.));
#11178=CARTESIAN_POINT('Origin',(9.,7.8995253021938,3.));
#11179=CARTESIAN_POINT('',(12.5,7.8995253021938,2.5));
#11180=CARTESIAN_POINT('',(9.,7.8995253021938,2.5));
#11181=CARTESIAN_POINT('',(12.5,7.43209776951961,2.82248520710059));
#11182=CARTESIAN_POINT('Origin',(12.5,7.8995253021938,3.));
#11183=CARTESIAN_POINT('',(9.,7.43209776951961,2.82248520710059));
#11184=CARTESIAN_POINT('Origin',(9.,8.62,2.5));
#11185=CARTESIAN_POINT('',(12.5,10.24,2.5));
#11186=CARTESIAN_POINT('',(14.,10.24,2.5));
#11187=CARTESIAN_POINT('',(12.5,8.285,2.5));
#11188=CARTESIAN_POINT('Origin',(14.,10.24,0.));
#11189=CARTESIAN_POINT('',(12.5,10.24,-2.5));
#11190=CARTESIAN_POINT('',(14.,10.24,-2.5));
#11191=CARTESIAN_POINT('',(12.5,10.24,0.));
#11192=CARTESIAN_POINT('Origin',(12.5,10.74,0.));
#11193=CARTESIAN_POINT('',(13.,10.74,-3.));
#11194=CARTESIAN_POINT('Origin',(12.5,10.74,-3.));
#11195=CARTESIAN_POINT('',(13.,10.74,3.));
#11196=CARTESIAN_POINT('',(13.,10.74,0.));
#11197=CARTESIAN_POINT('Origin',(12.5,10.74,3.));
#11198=CARTESIAN_POINT('Origin',(12.5,7.8995253021938,3.));
#11199=CARTESIAN_POINT('',(13.,7.8995253021938,3.));
#11200=CARTESIAN_POINT('Origin',(12.5,7.8995253021938,3.));
#11201=CARTESIAN_POINT('Origin',(12.5,7.8995253021938,3.));
#11202=CARTESIAN_POINT('Origin',(12.5,8.285,3.));
#11203=CARTESIAN_POINT('',(13.,8.285,3.));
#11204=CARTESIAN_POINT('Origin',(12.5,0.,0.));
#11205=CARTESIAN_POINT('',(13.,7.8995253021938,-3.));
#11206=CARTESIAN_POINT('Origin',(13.,0.,0.));
#11207=CARTESIAN_POINT('',(12.5,7.43209776951961,-2.82248520710059));
#11208=CARTESIAN_POINT('Origin',(12.5,7.8995253021938,-3.));
#11209=CARTESIAN_POINT('Origin',(12.5,0.,0.));
#11210=CARTESIAN_POINT('Origin',(12.5,0.,0.));
#11211=CARTESIAN_POINT('',(13.,-2.4440003129991E-15,19.9567770454363));
#11212=CARTESIAN_POINT('Origin',(13.,0.,0.));
#11213=CARTESIAN_POINT('',(12.9925825347358,-2.45450835807069E-15,20.0425817450355));
#11214=CARTESIAN_POINT('Origin',(12.5,-2.4440003129991E-15,19.9567770454363));
#11215=CARTESIAN_POINT('',(12.9925825347358,-20.0425817450355,-2.45450835807069E-15));
#11216=CARTESIAN_POINT('Origin',(12.9925825347358,0.,-3.06813544758836E-15));
#11217=CARTESIAN_POINT('Origin',(12.9925825347358,0.,-3.06813544758836E-15));
#11218=CARTESIAN_POINT('Origin',(13.,7.95,0.));
#11219=CARTESIAN_POINT('',(13.,8.285,-3.));
#11220=CARTESIAN_POINT('Origin',(10.3,0.,0.));
#11221=CARTESIAN_POINT('',(7.6,-51.,-6.2456986756515E-15));
#11222=CARTESIAN_POINT('',(10.3,-35.5,-4.3474961369731E-15));
#11223=CARTESIAN_POINT('',(7.6,51.,0.));
#11224=CARTESIAN_POINT('Origin',(7.6,0.,0.));
#11225=CARTESIAN_POINT('Origin',(7.6,0.,0.));
#11226=CARTESIAN_POINT('Origin',(5.5,7.8995253021938,-3.));
#11227=CARTESIAN_POINT('',(5.5,7.8995253021938,-2.5));
#11228=CARTESIAN_POINT('Origin',(5.5,7.8995253021938,-3.));
#11229=CARTESIAN_POINT('Origin',(5.5,7.8995253021938,-3.));
#11230=CARTESIAN_POINT('Origin',(5.5,10.31,-3.));
#11231=CARTESIAN_POINT('',(5.5,10.31,-2.5));
#11232=CARTESIAN_POINT('Origin',(9.,7.8995253021938,-3.));
#11233=CARTESIAN_POINT('',(12.5,7.8995253021938,-2.5));
#11234=CARTESIAN_POINT('Origin',(12.5,7.8995253021938,-3.));
#11235=CARTESIAN_POINT('',(9.,7.8995253021938,-2.5));
#11236=CARTESIAN_POINT('',(9.,7.43209776951961,-2.82248520710059));
#11237=CARTESIAN_POINT('Origin',(12.5,7.8995253021938,-3.));
#11238=CARTESIAN_POINT('Origin',(12.5,7.8995253021938,-3.));
#11239=CARTESIAN_POINT('Origin',(9.,8.62,-2.5));
#11240=CARTESIAN_POINT('',(12.5,8.285,-2.5));
#11241=CARTESIAN_POINT('Origin',(12.5,8.285,-3.));
#11242=CARTESIAN_POINT('Origin',(9.,0.,0.));
#11243=CARTESIAN_POINT('Ctrl Pts',(0.,56.8978458123625,2.49999999999978));
#11244=CARTESIAN_POINT('Ctrl Pts',(0.,56.5290913566253,10.8925336660656));
#11245=CARTESIAN_POINT('Ctrl Pts',(0.,52.0239399392849,27.5104427981014));
#11246=CARTESIAN_POINT('Ctrl Pts',(0.,37.0895128901808,44.9505513524534));
#11247=CARTESIAN_POINT('Ctrl Pts',(0.,19.6413066333793,54.3407718417784));
#11248=CARTESIAN_POINT('Ctrl Pts',(0.,2.98972976337264,57.7126473424414));
#11249=CARTESIAN_POINT('Ctrl Pts',(0.,-13.9100795010715,56.0762889490297));
#11250=CARTESIAN_POINT('Ctrl Pts',(0.,-34.8726547481504,47.4775611101652));
#11251=CARTESIAN_POINT('Ctrl Pts',(0.,-48.6578954952714,32.3601597542925));
#11252=CARTESIAN_POINT('Ctrl Pts',(0.,-54.6754985459398,16.615078371656));
#11253=CARTESIAN_POINT('Ctrl Pts',(0.,-58.4322800872165,0.182637285551057));
#11254=CARTESIAN_POINT('Ctrl Pts',(0.,-55.3972091422166,-20.0478023034309));
#11255=CARTESIAN_POINT('Ctrl Pts',(0.,-42.7587268357465,-38.8566003856648));
#11256=CARTESIAN_POINT('Ctrl Pts',(0.,-29.6277979733952,-49.6176180623964));
#11257=CARTESIAN_POINT('Ctrl Pts',(0.,-13.9134722149986,-56.083084294608));
#11258=CARTESIAN_POINT('Ctrl Pts',(0.,2.99163137042858,-57.710045079662));
#11259=CARTESIAN_POINT('Ctrl Pts',(0.,19.6409629692718,-54.3421091676748));
#11260=CARTESIAN_POINT('Ctrl Pts',(0.,37.0902013849514,-44.9493511994273));
#11261=CARTESIAN_POINT('Ctrl Pts',(0.,52.0238383479187,-27.5106172571882));
#11262=CARTESIAN_POINT('Ctrl Pts',(0.,56.5290913566252,-10.8925336660656));
#11263=CARTESIAN_POINT('Ctrl Pts',(0.,56.8978458123625,-2.49999999999977));
#11264=CARTESIAN_POINT('Ctrl Pts',(0.,57.001373876214,2.50454885691929));
#11265=CARTESIAN_POINT('Ctrl Pts',(-1.63742030236312E-19,56.6319480624753,
10.9123620526042));
#11266=CARTESIAN_POINT('Ctrl Pts',(9.48249132196878E-20,52.1186000182248,
27.5604934111569));
#11267=CARTESIAN_POINT('Ctrl Pts',(-1.19995263848322E-19,37.1569994229608,
45.0323427370933));
#11268=CARTESIAN_POINT('Ctrl Pts',(1.23050933331286E-19,19.6770452908852,
54.4396466559896));
#11269=CARTESIAN_POINT('Ctrl Pts',(-1.44052426172425E-19,2.9951686864826,
57.8176582375029));
#11270=CARTESIAN_POINT('Ctrl Pts',(3.14735156619693E-19,-13.935388031018,
56.1783232228821));
#11271=CARTESIAN_POINT('Ctrl Pts',(-6.67633563883309E-19,-34.9361090552895,
47.5639470777454));
#11272=CARTESIAN_POINT('Ctrl Pts',(1.58766279766169E-18,-48.746429713773,
32.4190424283386));
#11273=CARTESIAN_POINT('Ctrl Pts',(-1.26927833601234E-18,-54.774983220983,
16.645310295907));
#11274=CARTESIAN_POINT('Ctrl Pts',(4.57103728577927E-18,-58.5386002359852,
0.182968458669554));
#11275=CARTESIAN_POINT('Ctrl Pts',(-9.06026943189087E-18,-55.4980072978672,
-20.0842792997109));
#11276=CARTESIAN_POINT('Ctrl Pts',(1.1238606803883E-17,-42.8365283395576,
-38.9273017012347));
#11277=CARTESIAN_POINT('Ctrl Pts',(-3.02518942121921E-17,-29.68170664745,
-49.7079003853428));
#11278=CARTESIAN_POINT('Ctrl Pts',(1.07915148805084E-16,-13.9387883568906,
-56.1851293477377));
#11279=CARTESIAN_POINT('Ctrl Pts',(-2.95307104319226E-18,2.99707413713518,
-57.8150521907767));
#11280=CARTESIAN_POINT('Ctrl Pts',(2.05765094998786E-16,19.6767005375821,
-54.4409860649289));
#11281=CARTESIAN_POINT('Ctrl Pts',(-1.25774157565186E-16,37.1576897427545,
-45.0311405989928));
#11282=CARTESIAN_POINT('Ctrl Pts',(7.30652087057546E-17,52.1184978807484,
-27.5606680742516));
#11283=CARTESIAN_POINT('Ctrl Pts',(1.96124639940372E-19,56.6319480624753,
-10.9123620526041));
#11284=CARTESIAN_POINT('Ctrl Pts',(0.,57.001373876214,-2.50454885691928));
#11285=CARTESIAN_POINT('Ctrl Pts',(0.0667333574462435,57.2080172044309,
2.5136284330116));
#11286=CARTESIAN_POINT('Ctrl Pts',(0.0667333574462435,56.8372529234427,
10.9519039899706));
#11287=CARTESIAN_POINT('Ctrl Pts',(0.0667333574462479,52.3075415566464,
27.6604182942792));
#11288=CARTESIAN_POINT('Ctrl Pts',(0.066733357446241,37.2917010899539,45.1955916525164));
#11289=CARTESIAN_POINT('Ctrl Pts',(0.0667333574462441,19.7483782666853,
54.6370042126952));
#11290=CARTESIAN_POINT('Ctrl Pts',(0.066733357446246,3.00602891262606,58.0272602571566));
#11291=CARTESIAN_POINT('Ctrl Pts',(0.0667333574462456,-13.9859099881671,
56.3819806617786));
#11292=CARTESIAN_POINT('Ctrl Pts',(0.0667333574462422,-35.062756586454,
47.7363804977705));
#11293=CARTESIAN_POINT('Ctrl Pts',(0.066733357446249,-48.9231487449615,
32.5365650856458));
#11294=CARTESIAN_POINT('Ctrl Pts',(0.0667333574462432,-54.9735548269809,
16.7056532862401));
#11295=CARTESIAN_POINT('Ctrl Pts',(0.0667333574462437,-58.7508161372197,
0.183634051074929));
#11296=CARTESIAN_POINT('Ctrl Pts',(0.0667333574462451,-55.6991994401982,
-20.1570911918775));
#11297=CARTESIAN_POINT('Ctrl Pts',(0.0667333574462445,-42.991820442108,
-39.0684221465814));
#11298=CARTESIAN_POINT('Ctrl Pts',(0.0667333574462468,-29.789310528299,
-49.8881012725558));
#11299=CARTESIAN_POINT('Ctrl Pts',(0.0667333574462466,-13.9893197604443,
-56.3888146340892));
#11300=CARTESIAN_POINT('Ctrl Pts',(0.0667333574462478,3.00794050308572,
-58.0246428589159));
#11301=CARTESIAN_POINT('Ctrl Pts',(0.0667333574462471,19.7480331923249,
-54.6383491786078));
#11302=CARTESIAN_POINT('Ctrl Pts',(0.066733357446242,37.2923927665473,-45.1943847586508));
#11303=CARTESIAN_POINT('Ctrl Pts',(0.0667333574462439,52.3074397721863,
-27.6605938176656));
#11304=CARTESIAN_POINT('Ctrl Pts',(0.0667333574462471,56.8372529234427,
-10.9519039899706));
#11305=CARTESIAN_POINT('Ctrl Pts',(0.0667333574462471,57.2080172044309,
-2.51362843301159));
#11306=CARTESIAN_POINT('Ctrl Pts',(0.241146694675275,57.3375734782873,2.51932092769249));
#11307=CARTESIAN_POINT('Ctrl Pts',(0.241146694675275,56.9659668116783,10.9767684555204));
#11308=CARTESIAN_POINT('Ctrl Pts',(0.241146694675289,52.4260020076026,27.7230191395092));
#11309=CARTESIAN_POINT('Ctrl Pts',(0.241146694675268,37.3761578444925,45.2979573924083));
#11310=CARTESIAN_POINT('Ctrl Pts',(0.241146694675277,19.7931046748997,54.7607342556246));
#11311=CARTESIAN_POINT('Ctrl Pts',(0.241146694675283,3.01282945138884,58.1586736724148));
#11312=CARTESIAN_POINT('Ctrl Pts',(0.241146694675282,-14.0175731085778,
56.5096736677099));
#11313=CARTESIAN_POINT('Ctrl Pts',(0.241146694675271,-35.1421755770565,
47.8444764887727));
#11314=CARTESIAN_POINT('Ctrl Pts',(0.241146694675293,-49.0339363965306,
32.6102628457984));
#11315=CARTESIAN_POINT('Ctrl Pts',(0.241146694675275,-55.0980526755376,
16.7434863298973));
#11316=CARTESIAN_POINT('Ctrl Pts',(0.241146694675276,-58.8838671210771,
0.184041977005384));
#11317=CARTESIAN_POINT('Ctrl Pts',(0.241146694675281,-55.825342686821,-20.2027341799597));
#11318=CARTESIAN_POINT('Ctrl Pts',(0.241146694675279,-43.0891831640078,
-39.1568990246098));
#11319=CARTESIAN_POINT('Ctrl Pts',(0.241146694675286,-29.8567703816805,
-50.0010870444588));
#11320=CARTESIAN_POINT('Ctrl Pts',(0.241146694675285,-14.0210005969976,
-56.516512105534));
#11321=CARTESIAN_POINT('Ctrl Pts',(0.241146694675289,3.01474803516986,-58.1560569525823));
#11322=CARTESIAN_POINT('Ctrl Pts',(0.241146694675286,19.7927555967382,-54.7620798342382));
#11323=CARTESIAN_POINT('Ctrl Pts',(0.241146694675271,37.376855062764,-45.2967491452879));
#11324=CARTESIAN_POINT('Ctrl Pts',(0.241146694675276,52.4258974831749,-27.7231942724782));
#11325=CARTESIAN_POINT('Ctrl Pts',(0.241146694675286,56.9659668116783,-10.9767684555204));
#11326=CARTESIAN_POINT('Ctrl Pts',(0.241146694675286,57.3375734782873,-2.51932092769249));
#11327=CARTESIAN_POINT('Ctrl Pts',(0.339274733856657,57.370852629519,2.52078316017057));
#11328=CARTESIAN_POINT('Ctrl Pts',(0.339274733856657,56.9990326206148,10.9830861748047));
#11329=CARTESIAN_POINT('Ctrl Pts',(0.339274733856675,52.4564286898744,27.7391443737182));
#11330=CARTESIAN_POINT('Ctrl Pts',(0.339274733856648,37.397847805002,45.3242371558628));
#11331=CARTESIAN_POINT('Ctrl Pts',(0.339274733856659,19.8045900020693,54.7925210277751));
#11332=CARTESIAN_POINT('Ctrl Pts',(0.339274733856667,3.01458417638844,58.1924278198806));
#11333=CARTESIAN_POINT('Ctrl Pts',(0.339274733856666,-14.0257176651751,
56.5424659470342));
#11334=CARTESIAN_POINT('Ctrl Pts',(0.339274733856652,-35.162560335835,47.8722546129936));
#11335=CARTESIAN_POINT('Ctrl Pts',(0.33927473385668,-49.062401429532,32.6291783076228));
#11336=CARTESIAN_POINT('Ctrl Pts',(0.339274733856656,-55.130030403419,16.7532039056753));
#11337=CARTESIAN_POINT('Ctrl Pts',(0.339274733856658,-58.9180430616952,
0.184155597534577));
#11338=CARTESIAN_POINT('Ctrl Pts',(0.339274733856665,-55.8577407704635,
-20.2144649779688));
#11339=CARTESIAN_POINT('Ctrl Pts',(0.339274733856663,-43.114191423157,-39.1796255654678));
#11340=CARTESIAN_POINT('Ctrl Pts',(0.339274733856671,-29.8741016817107,
-50.03010242379));
#11341=CARTESIAN_POINT('Ctrl Pts',(0.339274733856671,-14.0291385836291,
-56.5493177841146));
#11342=CARTESIAN_POINT('Ctrl Pts',(0.339274733856675,3.01650159200602,-58.1898039238036));
#11343=CARTESIAN_POINT('Ctrl Pts',(0.339274733856671,19.8042434809913,-54.7938694712148));
#11344=CARTESIAN_POINT('Ctrl Pts',(0.339274733856652,37.3985420234115,-45.3230270256477));
#11345=CARTESIAN_POINT('Ctrl Pts',(0.339274733856658,52.4563262539523,-27.7393202831295));
#11346=CARTESIAN_POINT('Ctrl Pts',(0.339274733856671,56.9990326206148,-10.9830861748047));
#11347=CARTESIAN_POINT('Ctrl Pts',(0.339274733856672,57.370852629519,-2.52078316017056));
#11348=CARTESIAN_POINT('',(0.339274733856678,57.370852629519,-2.52078316017068));
#11349=CARTESIAN_POINT('Origin',(0.499999999999991,56.8978458123625,-2.49999999999977));
#11350=CARTESIAN_POINT('',(0.33927473385663,57.370852629519,2.52078316017068));
#11351=CARTESIAN_POINT('Ctrl Pts',(0.339274733856672,57.370852629519,-2.52078316017056));
#11352=CARTESIAN_POINT('Ctrl Pts',(0.339274733856671,56.9990326206148,-10.9830861748047));
#11353=CARTESIAN_POINT('Ctrl Pts',(0.339274733856658,52.4563262539523,-27.7393202831295));
#11354=CARTESIAN_POINT('Ctrl Pts',(0.339274733856652,37.3985420234115,-45.3230270256477));
#11355=CARTESIAN_POINT('Ctrl Pts',(0.339274733856671,19.8042434809913,-54.7938694712148));
#11356=CARTESIAN_POINT('Ctrl Pts',(0.339274733856675,3.01650159200602,-58.1898039238036));
#11357=CARTESIAN_POINT('Ctrl Pts',(0.339274733856671,-14.0291385836291,
-56.5493177841146));
#11358=CARTESIAN_POINT('Ctrl Pts',(0.339274733856671,-29.8741016817107,
-50.03010242379));
#11359=CARTESIAN_POINT('Ctrl Pts',(0.339274733856663,-43.114191423157,-39.1796255654678));
#11360=CARTESIAN_POINT('Ctrl Pts',(0.339274733856665,-55.8577407704635,
-20.2144649779688));
#11361=CARTESIAN_POINT('Ctrl Pts',(0.339274733856658,-58.9180430616952,
0.184155597534577));
#11362=CARTESIAN_POINT('Ctrl Pts',(0.339274733856656,-55.130030403419,16.7532039056753));
#11363=CARTESIAN_POINT('Ctrl Pts',(0.33927473385668,-49.062401429532,32.6291783076228));
#11364=CARTESIAN_POINT('Ctrl Pts',(0.339274733856652,-35.162560335835,47.8722546129936));
#11365=CARTESIAN_POINT('Ctrl Pts',(0.339274733856666,-14.0257176651751,
56.5424659470342));
#11366=CARTESIAN_POINT('Ctrl Pts',(0.339274733856667,3.01458417638844,58.1924278198806));
#11367=CARTESIAN_POINT('Ctrl Pts',(0.339274733856659,19.8045900020693,54.7925210277751));
#11368=CARTESIAN_POINT('Ctrl Pts',(0.339274733856648,37.397847805002,45.3242371558628));
#11369=CARTESIAN_POINT('Ctrl Pts',(0.339274733856675,52.4564286898744,27.7391443737182));
#11370=CARTESIAN_POINT('Ctrl Pts',(0.339274733856657,56.9990326206148,10.9830861748047));
#11371=CARTESIAN_POINT('Ctrl Pts',(0.339274733856657,57.370852629519,2.52078316017057));
#11372=CARTESIAN_POINT('Origin',(0.499999999999996,56.8978458123625,2.49999999999978));
#11373=CARTESIAN_POINT('Origin',(0.5,57.025,-2.5));
#11374=CARTESIAN_POINT('',(0.500000000000238,56.8978458123627,-2.));
#11375=CARTESIAN_POINT('',(0.5,57.025,-2.));
#11376=CARTESIAN_POINT('Origin',(0.5,56.8978458123627,-2.5));
#11377=CARTESIAN_POINT('Origin',(0.499999999999896,56.8978458123625,-2.50000000000002));
#11378=CARTESIAN_POINT('Origin',(0.499999999999896,56.8978458123625,-2.50000000000002));
#11379=CARTESIAN_POINT('Origin',(0.50000000000006,56.8978458123625,2.5));
#11380=CARTESIAN_POINT('Origin',(0.50000000000006,56.8978458123625,2.5));
#11381=CARTESIAN_POINT('Ctrl Pts',(3.30000000000023,57.2570611822017,2.));
#11382=CARTESIAN_POINT('Ctrl Pts',(2.35587473833117,57.3142929108325,2.));
#11383=CARTESIAN_POINT('Ctrl Pts',(1.39877068709439,57.1962523550954,2.));
#11384=CARTESIAN_POINT('Ctrl Pts',(0.499999999999973,56.8978458123625,2.));
#11385=CARTESIAN_POINT('Ctrl Pts',(3.31887371652615,57.5315882986027,1.99241789689239));
#11386=CARTESIAN_POINT('Ctrl Pts',(2.33276518160034,57.5906485008098,1.99241414329163));
#11387=CARTESIAN_POINT('Ctrl Pts',(1.35243127070208,57.4698597329915,1.99241931647724));
#11388=CARTESIAN_POINT('Ctrl Pts',(0.411584403188821,57.1580487103768,1.99244885315961));
#11389=CARTESIAN_POINT('Ctrl Pts',(3.33560242564919,57.7749152697563,2.24717484796588));
#11390=CARTESIAN_POINT('Ctrl Pts',(2.31227799847597,57.8355775691271,2.24725411917667));
#11391=CARTESIAN_POINT('Ctrl Pts',(1.3113738729421,57.7123824082935,2.24714501562381));
#11392=CARTESIAN_POINT('Ctrl Pts',(0.33317230266513,57.3888117943974,2.24652030369265));
#11393=CARTESIAN_POINT('Ctrl Pts',(3.33426151832809,57.7554111397819,2.52175932309878));
#11394=CARTESIAN_POINT('Ctrl Pts',(2.31390369740501,57.8158698649554,2.52187727319098));
#11395=CARTESIAN_POINT('Ctrl Pts',(1.31472805667249,57.6929865211876,2.52171535509758));
#11396=CARTESIAN_POINT('Ctrl Pts',(0.339274733856594,57.370852629519,2.52078316017079));
#11397=CARTESIAN_POINT('',(3.33426151832784,57.7554111397819,2.5217593230988));
#11398=CARTESIAN_POINT('Ctrl Pts',(0.339274733856594,57.370852629519,2.52078316017079));
#11399=CARTESIAN_POINT('Ctrl Pts',(1.31472805667249,57.6929865211876,2.52171535509758));
#11400=CARTESIAN_POINT('Ctrl Pts',(2.31390369740501,57.8158698649554,2.52187727319098));
#11401=CARTESIAN_POINT('Ctrl Pts',(3.33426151832809,57.7554111397819,2.52175932309878));
#11402=CARTESIAN_POINT('',(2.8,57.2767052616368,2.00002239837059));
#11403=CARTESIAN_POINT('Ctrl Pts',(2.8,57.2767052616368,2.00002239837057));
#11404=CARTESIAN_POINT('Ctrl Pts',(2.8,57.3233277916702,2.00046370280581));
#11405=CARTESIAN_POINT('Ctrl Pts',(2.80651496136854,57.3688442456262,2.00740850907209));
#11406=CARTESIAN_POINT('Ctrl Pts',(2.83278587942622,57.4609346234663,2.03422841201581));
#11407=CARTESIAN_POINT('Ctrl Pts',(2.85367658846432,57.5051794406759,2.0551738220974));
#11408=CARTESIAN_POINT('Ctrl Pts',(2.91264660817257,57.5950293001724,2.11357045087714));
#11409=CARTESIAN_POINT('Ctrl Pts',(2.95372899720548,57.6363582268879,2.15381041488786));
#11410=CARTESIAN_POINT('Ctrl Pts',(3.04719526219676,57.7037440534718,2.24472494887073));
#11411=CARTESIAN_POINT('Ctrl Pts',(3.10085066357071,57.7281426935397,2.29658544858127));
#11412=CARTESIAN_POINT('Ctrl Pts',(3.21310392137581,57.7576460364624,2.40487775337108));
#11413=CARTESIAN_POINT('Ctrl Pts',(3.27253044418014,57.7618592555108,2.46210260432533));
#11414=CARTESIAN_POINT('Ctrl Pts',(3.33207315475466,57.7556502890388,2.51964428176073));
#11415=CARTESIAN_POINT('Ctrl Pts',(3.33316746036322,57.7555325268421,2.52070188444643));
#11416=CARTESIAN_POINT('Ctrl Pts',(3.33426151832784,57.7554111397819,2.5217593230988));
#11417=CARTESIAN_POINT('Ctrl Pts',(2.79999999999999,57.2767052616368,2.00002239837056));
#11418=CARTESIAN_POINT('Ctrl Pts',(2.79999999999999,57.2751280778309,2.00000746957523));
#11419=CARTESIAN_POINT('Ctrl Pts',(2.79999999999993,57.273550476778,2.));
#11420=CARTESIAN_POINT('Ctrl Pts',(2.79999999999993,57.2719725101481,2.));
#11421=CARTESIAN_POINT('Ctrl Pts',(7.6,51.,0.));
#11422=CARTESIAN_POINT('Ctrl Pts',(7.6,51.,51.));
#11423=CARTESIAN_POINT('Ctrl Pts',(7.6,0.,51.));
#11424=CARTESIAN_POINT('Ctrl Pts',(7.6,-51.,51.));
#11425=CARTESIAN_POINT('Ctrl Pts',(7.6,-51.,0.));
#11426=CARTESIAN_POINT('Ctrl Pts',(7.6,-51.,-51.));
#11427=CARTESIAN_POINT('Ctrl Pts',(7.6,0.,-51.));
#11428=CARTESIAN_POINT('Ctrl Pts',(7.6,51.,-51.));
#11429=CARTESIAN_POINT('Ctrl Pts',(7.6,51.,0.));
#11430=CARTESIAN_POINT('Ctrl Pts',(7.59004574184823,51.1988330750386,0.));
#11431=CARTESIAN_POINT('Ctrl Pts',(7.59004574184823,51.1988330750386,51.1988330750386));
#11432=CARTESIAN_POINT('Ctrl Pts',(7.59004574184823,0.,51.1988330750386));
#11433=CARTESIAN_POINT('Ctrl Pts',(7.59004574184823,-51.1988330750386,51.1988330750386));
#11434=CARTESIAN_POINT('Ctrl Pts',(7.59004574184823,-51.1988330750386,0.));
#11435=CARTESIAN_POINT('Ctrl Pts',(7.59004574184823,-51.1988330750386,-51.1988330750386));
#11436=CARTESIAN_POINT('Ctrl Pts',(7.59004574184823,0.,-51.1988330750386));
#11437=CARTESIAN_POINT('Ctrl Pts',(7.59004574184823,51.1988330750386,-51.1988330750386));
#11438=CARTESIAN_POINT('Ctrl Pts',(7.59004574184823,51.1988330750386,0.));
#11439=CARTESIAN_POINT('Ctrl Pts',(7.56669216920305,51.5895935047463,0.));
#11440=CARTESIAN_POINT('Ctrl Pts',(7.56669216920305,51.5895935047463,51.5895935047463));
#11441=CARTESIAN_POINT('Ctrl Pts',(7.56669216920305,0.,51.5895935047463));
#11442=CARTESIAN_POINT('Ctrl Pts',(7.56669216920305,-51.5895935047463,51.5895935047463));
#11443=CARTESIAN_POINT('Ctrl Pts',(7.56669216920305,-51.5895935047463,0.));
#11444=CARTESIAN_POINT('Ctrl Pts',(7.56669216920305,-51.5895935047463,-51.5895935047463));
#11445=CARTESIAN_POINT('Ctrl Pts',(7.56669216920305,0.,-51.5895935047463));
#11446=CARTESIAN_POINT('Ctrl Pts',(7.56669216920305,51.5895935047463,-51.5895935047463));
#11447=CARTESIAN_POINT('Ctrl Pts',(7.56669216920305,51.5895935047463,0.));
#11448=CARTESIAN_POINT('Ctrl Pts',(7.52132668197793,52.1550170184989,0.));
#11449=CARTESIAN_POINT('Ctrl Pts',(7.52132668197793,52.1550170184989,52.1550170184989));
#11450=CARTESIAN_POINT('Ctrl Pts',(7.52132668197793,0.,52.1550170184989));
#11451=CARTESIAN_POINT('Ctrl Pts',(7.52132668197793,-52.1550170184989,52.1550170184989));
#11452=CARTESIAN_POINT('Ctrl Pts',(7.52132668197793,-52.1550170184989,0.));
#11453=CARTESIAN_POINT('Ctrl Pts',(7.52132668197793,-52.1550170184989,-52.1550170184989));
#11454=CARTESIAN_POINT('Ctrl Pts',(7.52132668197793,0.,-52.1550170184989));
#11455=CARTESIAN_POINT('Ctrl Pts',(7.52132668197793,52.1550170184989,-52.1550170184989));
#11456=CARTESIAN_POINT('Ctrl Pts',(7.52132668197793,52.1550170184989,0.));
#11457=CARTESIAN_POINT('Ctrl Pts',(7.4400844252614,52.8673114594784,0.));
#11458=CARTESIAN_POINT('Ctrl Pts',(7.4400844252614,52.8673114594784,52.8673114594784));
#11459=CARTESIAN_POINT('Ctrl Pts',(7.4400844252614,0.,52.8673114594784));
#11460=CARTESIAN_POINT('Ctrl Pts',(7.4400844252614,-52.8673114594784,52.8673114594784));
#11461=CARTESIAN_POINT('Ctrl Pts',(7.4400844252614,-52.8673114594784,0.));
#11462=CARTESIAN_POINT('Ctrl Pts',(7.4400844252614,-52.8673114594784,-52.8673114594784));
#11463=CARTESIAN_POINT('Ctrl Pts',(7.4400844252614,0.,-52.8673114594784));
#11464=CARTESIAN_POINT('Ctrl Pts',(7.4400844252614,52.8673114594784,-52.8673114594784));
#11465=CARTESIAN_POINT('Ctrl Pts',(7.4400844252614,52.8673114594784,0.));
#11466=CARTESIAN_POINT('Ctrl Pts',(7.303261488895,53.6872261791492,0.));
#11467=CARTESIAN_POINT('Ctrl Pts',(7.303261488895,53.6872261791492,53.6872261791492));
#11468=CARTESIAN_POINT('Ctrl Pts',(7.303261488895,0.,53.6872261791492));
#11469=CARTESIAN_POINT('Ctrl Pts',(7.303261488895,-53.6872261791492,53.6872261791492));
#11470=CARTESIAN_POINT('Ctrl Pts',(7.303261488895,-53.6872261791492,0.));
#11471=CARTESIAN_POINT('Ctrl Pts',(7.303261488895,-53.6872261791492,-53.6872261791492));
#11472=CARTESIAN_POINT('Ctrl Pts',(7.303261488895,0.,-53.6872261791492));
#11473=CARTESIAN_POINT('Ctrl Pts',(7.303261488895,53.6872261791492,-53.6872261791492));
#11474=CARTESIAN_POINT('Ctrl Pts',(7.303261488895,53.6872261791492,0.));
#11475=CARTESIAN_POINT('Ctrl Pts',(7.1299954347016,54.4350859396526,0.));
#11476=CARTESIAN_POINT('Ctrl Pts',(7.1299954347016,54.4350859396526,54.4350859396526));
#11477=CARTESIAN_POINT('Ctrl Pts',(7.1299954347016,0.,54.4350859396526));
#11478=CARTESIAN_POINT('Ctrl Pts',(7.1299954347016,-54.4350859396526,54.4350859396526));
#11479=CARTESIAN_POINT('Ctrl Pts',(7.1299954347016,-54.4350859396526,0.));
#11480=CARTESIAN_POINT('Ctrl Pts',(7.1299954347016,-54.4350859396526,-54.4350859396526));
#11481=CARTESIAN_POINT('Ctrl Pts',(7.1299954347016,0.,-54.4350859396526));
#11482=CARTESIAN_POINT('Ctrl Pts',(7.1299954347016,54.4350859396526,-54.4350859396526));
#11483=CARTESIAN_POINT('Ctrl Pts',(7.1299954347016,54.4350859396526,0.));
#11484=CARTESIAN_POINT('Ctrl Pts',(6.91862269230318,55.1090497640848,0.));
#11485=CARTESIAN_POINT('Ctrl Pts',(6.91862269230318,55.1090497640848,55.1090497640848));
#11486=CARTESIAN_POINT('Ctrl Pts',(6.91862269230318,0.,55.1090497640848));
#11487=CARTESIAN_POINT('Ctrl Pts',(6.91862269230318,-55.1090497640848,55.1090497640848));
#11488=CARTESIAN_POINT('Ctrl Pts',(6.91862269230318,-55.1090497640848,0.));
#11489=CARTESIAN_POINT('Ctrl Pts',(6.91862269230318,-55.1090497640848,-55.1090497640848));
#11490=CARTESIAN_POINT('Ctrl Pts',(6.91862269230318,0.,-55.1090497640848));
#11491=CARTESIAN_POINT('Ctrl Pts',(6.91862269230318,55.1090497640848,-55.1090497640848));
#11492=CARTESIAN_POINT('Ctrl Pts',(6.91862269230318,55.1090497640848,0.));
#11493=CARTESIAN_POINT('Ctrl Pts',(6.66699410333038,55.7073490432259,0.));
#11494=CARTESIAN_POINT('Ctrl Pts',(6.66699410333038,55.7073490432258,55.7073490432258));
#11495=CARTESIAN_POINT('Ctrl Pts',(6.66699410333038,0.,55.7073490432259));
#11496=CARTESIAN_POINT('Ctrl Pts',(6.66699410333038,-55.7073490432258,55.7073490432258));
#11497=CARTESIAN_POINT('Ctrl Pts',(6.66699410333038,-55.7073490432259,0.));
#11498=CARTESIAN_POINT('Ctrl Pts',(6.66699410333038,-55.7073490432258,-55.7073490432258));
#11499=CARTESIAN_POINT('Ctrl Pts',(6.66699410333038,0.,-55.7073490432259));
#11500=CARTESIAN_POINT('Ctrl Pts',(6.66699410333038,55.7073490432258,-55.7073490432258));
#11501=CARTESIAN_POINT('Ctrl Pts',(6.66699410333038,55.7073490432259,0.));
#11502=CARTESIAN_POINT('Ctrl Pts',(6.37255361362915,56.2286342531435,0.));
#11503=CARTESIAN_POINT('Ctrl Pts',(6.37255361362915,56.2286342531435,56.2286342531435));
#11504=CARTESIAN_POINT('Ctrl Pts',(6.37255361362915,0.,56.2286342531435));
#11505=CARTESIAN_POINT('Ctrl Pts',(6.37255361362915,-56.2286342531435,56.2286342531435));
#11506=CARTESIAN_POINT('Ctrl Pts',(6.37255361362915,-56.2286342531435,0.));
#11507=CARTESIAN_POINT('Ctrl Pts',(6.37255361362915,-56.2286342531435,-56.2286342531435));
#11508=CARTESIAN_POINT('Ctrl Pts',(6.37255361362915,0.,-56.2286342531435));
#11509=CARTESIAN_POINT('Ctrl Pts',(6.37255361362915,56.2286342531435,-56.2286342531435));
#11510=CARTESIAN_POINT('Ctrl Pts',(6.37255361362915,56.2286342531435,0.));
#11511=CARTESIAN_POINT('Ctrl Pts',(6.03231545780073,56.6724462969604,0.));
#11512=CARTESIAN_POINT('Ctrl Pts',(6.03231545780073,56.6724462969604,56.6724462969604));
#11513=CARTESIAN_POINT('Ctrl Pts',(6.03231545780073,0.,56.6724462969604));
#11514=CARTESIAN_POINT('Ctrl Pts',(6.03231545780073,-56.6724462969604,56.6724462969604));
#11515=CARTESIAN_POINT('Ctrl Pts',(6.03231545780073,-56.6724462969604,0.));
#11516=CARTESIAN_POINT('Ctrl Pts',(6.03231545780073,-56.6724462969604,-56.6724462969604));
#11517=CARTESIAN_POINT('Ctrl Pts',(6.03231545780073,0.,-56.6724462969604));
#11518=CARTESIAN_POINT('Ctrl Pts',(6.03231545780073,56.6724462969604,-56.6724462969604));
#11519=CARTESIAN_POINT('Ctrl Pts',(6.03231545780073,56.6724462969604,0.));
#11520=CARTESIAN_POINT('Ctrl Pts',(5.64378712881462,57.0393576788909,0.));
#11521=CARTESIAN_POINT('Ctrl Pts',(5.64378712881462,57.0393576788909,57.0393576788909));
#11522=CARTESIAN_POINT('Ctrl Pts',(5.64378712881462,0.,57.0393576788909));
#11523=CARTESIAN_POINT('Ctrl Pts',(5.64378712881462,-57.0393576788909,57.0393576788909));
#11524=CARTESIAN_POINT('Ctrl Pts',(5.64378712881462,-57.0393576788909,0.));
#11525=CARTESIAN_POINT('Ctrl Pts',(5.64378712881462,-57.0393576788909,-57.0393576788909));
#11526=CARTESIAN_POINT('Ctrl Pts',(5.64378712881462,0.,-57.0393576788909));
#11527=CARTESIAN_POINT('Ctrl Pts',(5.64378712881462,57.0393576788909,-57.0393576788909));
#11528=CARTESIAN_POINT('Ctrl Pts',(5.64378712881462,57.0393576788909,0.));
#11529=CARTESIAN_POINT('Ctrl Pts',(5.20620249661537,57.331109156058,0.));
#11530=CARTESIAN_POINT('Ctrl Pts',(5.20620249661537,57.331109156058,57.331109156058));
#11531=CARTESIAN_POINT('Ctrl Pts',(5.20620249661537,0.,57.331109156058));
#11532=CARTESIAN_POINT('Ctrl Pts',(5.20620249661537,-57.331109156058,57.331109156058));
#11533=CARTESIAN_POINT('Ctrl Pts',(5.20620249661537,-57.331109156058,0.));
#11534=CARTESIAN_POINT('Ctrl Pts',(5.20620249661537,-57.331109156058,-57.331109156058));
#11535=CARTESIAN_POINT('Ctrl Pts',(5.20620249661537,0.,-57.331109156058));
#11536=CARTESIAN_POINT('Ctrl Pts',(5.20620249661537,57.331109156058,-57.331109156058));
#11537=CARTESIAN_POINT('Ctrl Pts',(5.20620249661537,57.331109156058,0.));
#11538=CARTESIAN_POINT('Ctrl Pts',(4.72163375439117,57.5508140869366,0.));
#11539=CARTESIAN_POINT('Ctrl Pts',(4.72163375439117,57.5508140869366,57.5508140869366));
#11540=CARTESIAN_POINT('Ctrl Pts',(4.72163375439117,0.,57.5508140869366));
#11541=CARTESIAN_POINT('Ctrl Pts',(4.72163375439117,-57.5508140869366,57.5508140869366));
#11542=CARTESIAN_POINT('Ctrl Pts',(4.72163375439117,-57.5508140869366,0.));
#11543=CARTESIAN_POINT('Ctrl Pts',(4.72163375439117,-57.5508140869366,-57.5508140869366));
#11544=CARTESIAN_POINT('Ctrl Pts',(4.72163375439117,0.,-57.5508140869366));
#11545=CARTESIAN_POINT('Ctrl Pts',(4.72163375439117,57.5508140869366,-57.5508140869366));
#11546=CARTESIAN_POINT('Ctrl Pts',(4.72163375439117,57.5508140869366,0.));
#11547=CARTESIAN_POINT('Ctrl Pts',(4.19645380044969,57.7033168044223,0.));
#11548=CARTESIAN_POINT('Ctrl Pts',(4.19645380044969,57.7033168044223,57.7033168044223));
#11549=CARTESIAN_POINT('Ctrl Pts',(4.19645380044969,0.,57.7033168044223));
#11550=CARTESIAN_POINT('Ctrl Pts',(4.19645380044969,-57.7033168044223,57.7033168044223));
#11551=CARTESIAN_POINT('Ctrl Pts',(4.19645380044969,-57.7033168044223,0.));
#11552=CARTESIAN_POINT('Ctrl Pts',(4.19645380044969,-57.7033168044223,-57.7033168044223));
#11553=CARTESIAN_POINT('Ctrl Pts',(4.19645380044969,0.,-57.7033168044223));
#11554=CARTESIAN_POINT('Ctrl Pts',(4.19645380044969,57.7033168044223,-57.7033168044223));
#11555=CARTESIAN_POINT('Ctrl Pts',(4.19645380044969,57.7033168044223,0.));
#11556=CARTESIAN_POINT('Ctrl Pts',(3.64216788966644,57.7953691453965,0.));
#11557=CARTESIAN_POINT('Ctrl Pts',(3.64216788966644,57.7953691453965,57.7953691453965));
#11558=CARTESIAN_POINT('Ctrl Pts',(3.64216788966644,0.,57.7953691453965));
#11559=CARTESIAN_POINT('Ctrl Pts',(3.64216788966644,-57.7953691453965,57.7953691453965));
#11560=CARTESIAN_POINT('Ctrl Pts',(3.64216788966644,-57.7953691453965,0.));
#11561=CARTESIAN_POINT('Ctrl Pts',(3.64216788966644,-57.7953691453965,-57.7953691453965));
#11562=CARTESIAN_POINT('Ctrl Pts',(3.64216788966644,0.,-57.7953691453965));
#11563=CARTESIAN_POINT('Ctrl Pts',(3.64216788966644,57.7953691453965,-57.7953691453965));
#11564=CARTESIAN_POINT('Ctrl Pts',(3.64216788966644,57.7953691453965,0.));
#11565=CARTESIAN_POINT('Ctrl Pts',(3.07295993429612,57.8346034867151,0.));
#11566=CARTESIAN_POINT('Ctrl Pts',(3.07295993429612,57.8346034867151,57.8346034867151));
#11567=CARTESIAN_POINT('Ctrl Pts',(3.07295993429612,0.,57.8346034867151));
#11568=CARTESIAN_POINT('Ctrl Pts',(3.07295993429612,-57.8346034867151,57.8346034867151));
#11569=CARTESIAN_POINT('Ctrl Pts',(3.07295993429612,-57.8346034867151,0.));
#11570=CARTESIAN_POINT('Ctrl Pts',(3.07295993429612,-57.8346034867151,-57.8346034867151));
#11571=CARTESIAN_POINT('Ctrl Pts',(3.07295993429612,0.,-57.8346034867151));
#11572=CARTESIAN_POINT('Ctrl Pts',(3.07295993429612,57.8346034867151,-57.8346034867151));
#11573=CARTESIAN_POINT('Ctrl Pts',(3.07295993429612,57.8346034867151,0.));
#11574=CARTESIAN_POINT('Ctrl Pts',(2.50364225081115,57.8287013224614,0.));
#11575=CARTESIAN_POINT('Ctrl Pts',(2.50364225081115,57.8287013224614,57.8287013224614));
#11576=CARTESIAN_POINT('Ctrl Pts',(2.50364225081115,0.,57.8287013224614));
#11577=CARTESIAN_POINT('Ctrl Pts',(2.50364225081115,-57.8287013224614,57.8287013224614));
#11578=CARTESIAN_POINT('Ctrl Pts',(2.50364225081115,-57.8287013224614,0.));
#11579=CARTESIAN_POINT('Ctrl Pts',(2.50364225081115,-57.8287013224614,-57.8287013224614));
#11580=CARTESIAN_POINT('Ctrl Pts',(2.50364225081115,0.,-57.8287013224614));
#11581=CARTESIAN_POINT('Ctrl Pts',(2.50364225081115,57.8287013224614,-57.8287013224614));
#11582=CARTESIAN_POINT('Ctrl Pts',(2.50364225081115,57.8287013224614,0.));
#11583=CARTESIAN_POINT('Ctrl Pts',(1.94767564770796,57.7846117731639,0.));
#11584=CARTESIAN_POINT('Ctrl Pts',(1.94767564770796,57.7846117731638,57.7846117731638));
#11585=CARTESIAN_POINT('Ctrl Pts',(1.94767564770796,0.,57.7846117731639));
#11586=CARTESIAN_POINT('Ctrl Pts',(1.94767564770796,-57.7846117731638,57.7846117731638));
#11587=CARTESIAN_POINT('Ctrl Pts',(1.94767564770796,-57.7846117731639,0.));
#11588=CARTESIAN_POINT('Ctrl Pts',(1.94767564770796,-57.7846117731638,-57.7846117731638));
#11589=CARTESIAN_POINT('Ctrl Pts',(1.94767564770796,0.,-57.7846117731639));
#11590=CARTESIAN_POINT('Ctrl Pts',(1.94767564770796,57.7846117731638,-57.7846117731638));
#11591=CARTESIAN_POINT('Ctrl Pts',(1.94767564770796,57.7846117731639,0.));
#11592=CARTESIAN_POINT('Ctrl Pts',(1.41470323398176,57.7076450358389,0.));
#11593=CARTESIAN_POINT('Ctrl Pts',(1.41470323398176,57.7076450358389,57.7076450358389));
#11594=CARTESIAN_POINT('Ctrl Pts',(1.41470323398176,0.,57.7076450358389));
#11595=CARTESIAN_POINT('Ctrl Pts',(1.41470323398176,-57.7076450358389,57.7076450358389));
#11596=CARTESIAN_POINT('Ctrl Pts',(1.41470323398176,-57.7076450358389,0.));
#11597=CARTESIAN_POINT('Ctrl Pts',(1.41470323398176,-57.7076450358389,-57.7076450358389));
#11598=CARTESIAN_POINT('Ctrl Pts',(1.41470323398176,0.,-57.7076450358389));
#11599=CARTESIAN_POINT('Ctrl Pts',(1.41470323398176,57.7076450358389,-57.7076450358389));
#11600=CARTESIAN_POINT('Ctrl Pts',(1.41470323398176,57.7076450358389,0.));
#11601=CARTESIAN_POINT('Ctrl Pts',(0.909896369306813,57.6011916129045,0.));
#11602=CARTESIAN_POINT('Ctrl Pts',(0.909896369306813,57.6011916129045,57.6011916129045));
#11603=CARTESIAN_POINT('Ctrl Pts',(0.909896369306813,0.,57.6011916129045));
#11604=CARTESIAN_POINT('Ctrl Pts',(0.909896369306813,-57.6011916129045,
57.6011916129045));
#11605=CARTESIAN_POINT('Ctrl Pts',(0.909896369306813,-57.6011916129045,
0.));
#11606=CARTESIAN_POINT('Ctrl Pts',(0.909896369306813,-57.6011916129045,
-57.6011916129045));
#11607=CARTESIAN_POINT('Ctrl Pts',(0.909896369306813,0.,-57.6011916129045));
#11608=CARTESIAN_POINT('Ctrl Pts',(0.909896369306813,57.6011916129045,-57.6011916129045));
#11609=CARTESIAN_POINT('Ctrl Pts',(0.909896369306813,57.6011916129045,0.));
#11610=CARTESIAN_POINT('Ctrl Pts',(0.530456882251734,57.4940201174365,0.));
#11611=CARTESIAN_POINT('Ctrl Pts',(0.530456882251734,57.4940201174365,57.4940201174365));
#11612=CARTESIAN_POINT('Ctrl Pts',(0.530456882251733,0.,57.4940201174365));
#11613=CARTESIAN_POINT('Ctrl Pts',(0.530456882251732,-57.4940201174365,
57.4940201174365));
#11614=CARTESIAN_POINT('Ctrl Pts',(0.530456882251732,-57.4940201174365,
0.));
#11615=CARTESIAN_POINT('Ctrl Pts',(0.530456882251732,-57.4940201174365,
-57.4940201174365));
#11616=CARTESIAN_POINT('Ctrl Pts',(0.530456882251733,0.,-57.4940201174365));
#11617=CARTESIAN_POINT('Ctrl Pts',(0.530456882251734,57.4940201174365,-57.4940201174365));
#11618=CARTESIAN_POINT('Ctrl Pts',(0.530456882251734,57.4940201174365,0.));
#11619=CARTESIAN_POINT('Ctrl Pts',(0.25982504671998,57.4016528748871,0.));
#11620=CARTESIAN_POINT('Ctrl Pts',(0.25982504671998,57.4016528748871,57.4016528748871));
#11621=CARTESIAN_POINT('Ctrl Pts',(0.259825046719979,0.,57.4016528748871));
#11622=CARTESIAN_POINT('Ctrl Pts',(0.259825046719979,-57.4016528748871,
57.4016528748871));
#11623=CARTESIAN_POINT('Ctrl Pts',(0.259825046719979,-57.4016528748871,
0.));
#11624=CARTESIAN_POINT('Ctrl Pts',(0.259825046719979,-57.4016528748871,
-57.4016528748871));
#11625=CARTESIAN_POINT('Ctrl Pts',(0.259825046719979,0.,-57.4016528748871));
#11626=CARTESIAN_POINT('Ctrl Pts',(0.25982504671998,57.4016528748871,-57.4016528748871));
#11627=CARTESIAN_POINT('Ctrl Pts',(0.25982504671998,57.4016528748871,0.));
#11628=CARTESIAN_POINT('Ctrl Pts',(0.0855791821307019,57.3347686565506,
0.));
#11629=CARTESIAN_POINT('Ctrl Pts',(0.0855791821307019,57.3347686565505,
57.3347686565505));
#11630=CARTESIAN_POINT('Ctrl Pts',(0.0855791821307017,0.,57.3347686565506));
#11631=CARTESIAN_POINT('Ctrl Pts',(0.0855791821307015,-57.3347686565505,
57.3347686565505));
#11632=CARTESIAN_POINT('Ctrl Pts',(0.0855791821307015,-57.3347686565506,
0.));
#11633=CARTESIAN_POINT('Ctrl Pts',(0.0855791821307015,-57.3347686565505,
-57.3347686565505));
#11634=CARTESIAN_POINT('Ctrl Pts',(0.0855791821307017,0.,-57.3347686565506));
#11635=CARTESIAN_POINT('Ctrl Pts',(0.0855791821307019,57.3347686565505,
-57.3347686565505));
#11636=CARTESIAN_POINT('Ctrl Pts',(0.0855791821307019,57.3347686565506,
0.));
#11637=CARTESIAN_POINT('Ctrl Pts',(0.,57.3,0.));
#11638=CARTESIAN_POINT('Ctrl Pts',(0.,57.3,57.3));
#11639=CARTESIAN_POINT('Ctrl Pts',(0.,0.,57.3));
#11640=CARTESIAN_POINT('Ctrl Pts',(0.,-57.3,57.3));
#11641=CARTESIAN_POINT('Ctrl Pts',(0.,-57.3,0.));
#11642=CARTESIAN_POINT('Ctrl Pts',(0.,-57.3,-57.3));
#11643=CARTESIAN_POINT('Ctrl Pts',(0.,0.,-57.3));
#11644=CARTESIAN_POINT('Ctrl Pts',(0.,57.3,-57.3));
#11645=CARTESIAN_POINT('Ctrl Pts',(0.,57.3,0.));
#11646=CARTESIAN_POINT('',(3.33426151832784,57.7554111397819,-2.5217593230988));
#11647=CARTESIAN_POINT('Ctrl Pts',(3.33426151832794,57.7554111397819,-2.5217593230988));
#11648=CARTESIAN_POINT('Ctrl Pts',(2.31390369740531,57.8158698649553,-2.52187727319098));
#11649=CARTESIAN_POINT('Ctrl Pts',(1.31472805667171,57.6929865211876,-2.52171535509756));
#11650=CARTESIAN_POINT('Ctrl Pts',(0.339274733856492,57.3708526295189,-2.52078316017081));
#11651=CARTESIAN_POINT('',(3.33426151832786,57.8104383827772,4.21884749357559E-14));
#11652=CARTESIAN_POINT('Ctrl Pts',(3.33426151832784,57.8104299775689,8.7513329916078E-12));
#11653=CARTESIAN_POINT('Ctrl Pts',(3.33426151832784,57.8104299773062,-0.840857117582111));
#11654=CARTESIAN_POINT('Ctrl Pts',(3.33426151832784,57.792090085957,-1.68170785699931));
#11655=CARTESIAN_POINT('Ctrl Pts',(3.33426151832784,57.7554111397819,-2.5217593230989));
#11656=CARTESIAN_POINT('Ctrl Pts',(3.33426151832786,57.8104383827772,0.));
#11657=CARTESIAN_POINT('Ctrl Pts',(3.39537650339183,57.8062407319816,0.));
#11658=CARTESIAN_POINT('Ctrl Pts',(3.56948527592296,57.7922402732231,0.));
#11659=CARTESIAN_POINT('Ctrl Pts',(3.85481788311223,57.7593613281302,0.));
#11660=CARTESIAN_POINT('Ctrl Pts',(4.24482380713023,57.6892710332381,0.));
#11661=CARTESIAN_POINT('Ctrl Pts',(4.72163375439117,57.5508140869366,0.));
#11662=CARTESIAN_POINT('Ctrl Pts',(5.20620249661537,57.331109156058,0.));
#11663=CARTESIAN_POINT('Ctrl Pts',(5.64378712881462,57.0393576788909,0.));
#11664=CARTESIAN_POINT('Ctrl Pts',(6.03231545780073,56.6724462969604,0.));
#11665=CARTESIAN_POINT('Ctrl Pts',(6.37255361362915,56.2286342531435,0.));
#11666=CARTESIAN_POINT('Ctrl Pts',(6.66699410333038,55.7073490432259,0.));
#11667=CARTESIAN_POINT('Ctrl Pts',(6.91862269230318,55.1090497640848,0.));
#11668=CARTESIAN_POINT('Ctrl Pts',(7.1299954347016,54.4350859396526,0.));
#11669=CARTESIAN_POINT('Ctrl Pts',(7.303261488895,53.6872261791492,0.));
#11670=CARTESIAN_POINT('Ctrl Pts',(7.4400844252614,52.8673114594784,0.));
#11671=CARTESIAN_POINT('Ctrl Pts',(7.52132668197793,52.1550170184989,0.));
#11672=CARTESIAN_POINT('Ctrl Pts',(7.56669216920305,51.5895935047463,0.));
#11673=CARTESIAN_POINT('Ctrl Pts',(7.59004574184823,51.1988330750386,0.));
#11674=CARTESIAN_POINT('Ctrl Pts',(7.6,51.,0.));
#11675=CARTESIAN_POINT('Ctrl Pts',(3.33426151832784,57.7554111397819,2.5217593230988));
#11676=CARTESIAN_POINT('Ctrl Pts',(3.33426151832784,57.7920906439767,1.68169507677206));
#11677=CARTESIAN_POINT('Ctrl Pts',(3.33426151832784,57.8104299778316,0.840844349400496));
#11678=CARTESIAN_POINT('Ctrl Pts',(3.33426151832784,57.8104299775689,8.89477380638937E-12));
#11679=CARTESIAN_POINT('Ctrl Pts',(0.499999999999865,56.8978458123625,-2.));
#11680=CARTESIAN_POINT('Ctrl Pts',(1.39877068709361,57.1962523550952,-2.));
#11681=CARTESIAN_POINT('Ctrl Pts',(2.35587473833157,57.3142929108325,-2.));
#11682=CARTESIAN_POINT('Ctrl Pts',(3.30000000000009,57.2570611822017,-2.));
#11683=CARTESIAN_POINT('Ctrl Pts',(0.411584403188717,57.1580487103768,-1.99244885315961));
#11684=CARTESIAN_POINT('Ctrl Pts',(1.3524312707013,57.4698597329914,-1.99241931647723));
#11685=CARTESIAN_POINT('Ctrl Pts',(2.33276518160068,57.5906485008099,-1.99241414329164));
#11686=CARTESIAN_POINT('Ctrl Pts',(3.318873716526,57.5315882986027,-1.99241789689239));
#11687=CARTESIAN_POINT('Ctrl Pts',(0.333172302665028,57.3888117943974,-2.24652030369265));
#11688=CARTESIAN_POINT('Ctrl Pts',(1.31137387294133,57.7123824082932,-2.24714501562381));
#11689=CARTESIAN_POINT('Ctrl Pts',(2.31227799847626,57.8355775691272,-2.24725411917667));
#11690=CARTESIAN_POINT('Ctrl Pts',(3.33560242564904,57.7749152697564,-2.24717484796589));
#11691=CARTESIAN_POINT('Ctrl Pts',(0.339274733856492,57.3708526295189,-2.52078316017081));
#11692=CARTESIAN_POINT('Ctrl Pts',(1.31472805667171,57.6929865211876,-2.52171535509756));
#11693=CARTESIAN_POINT('Ctrl Pts',(2.31390369740531,57.8158698649553,-2.52187727319098));
#11694=CARTESIAN_POINT('Ctrl Pts',(3.33426151832794,57.7554111397819,-2.5217593230988));
#11695=CARTESIAN_POINT('',(2.80000000000039,57.2719725101482,-2.));
#11696=CARTESIAN_POINT('Ctrl Pts',(0.499999999999865,56.8978458123625,-2.));
#11697=CARTESIAN_POINT('Ctrl Pts',(1.24037244163541,57.1436615513665,-2.));
#11698=CARTESIAN_POINT('Ctrl Pts',(2.02032888654137,57.267084078118,-2.));
#11699=CARTESIAN_POINT('Ctrl Pts',(2.80000655418616,57.2709607214293,-2.));
#11700=CARTESIAN_POINT('',(2.8,57.2767052616367,-2.00002239837057));
#11701=CARTESIAN_POINT('Ctrl Pts',(2.8,57.2719725101481,-2.));
#11702=CARTESIAN_POINT('Ctrl Pts',(2.8,57.2735503201058,-2.));
#11703=CARTESIAN_POINT('Ctrl Pts',(2.8,57.2751279214594,-2.0000074680951));
#11704=CARTESIAN_POINT('Ctrl Pts',(2.8,57.2767052616367,-2.00002239837056));
#11705=CARTESIAN_POINT('Ctrl Pts',(2.8,57.2767052616367,-2.00002239837056));
#11706=CARTESIAN_POINT('Ctrl Pts',(2.8,57.3233277916701,-2.0004637028058));
#11707=CARTESIAN_POINT('Ctrl Pts',(2.80651496136847,57.3688442456259,-2.00740850907196));
#11708=CARTESIAN_POINT('Ctrl Pts',(2.83278587942598,57.4609346234655,-2.03422841201549));
#11709=CARTESIAN_POINT('Ctrl Pts',(2.85367658846371,57.5051794406747,-2.05517382209671));
#11710=CARTESIAN_POINT('Ctrl Pts',(2.91264660817062,57.5950293001698,-2.11357045087513));
#11711=CARTESIAN_POINT('Ctrl Pts',(2.95372899720229,57.6363582268848,-2.15381041488474));
#11712=CARTESIAN_POINT('Ctrl Pts',(3.04719526219418,57.7037440534708,-2.24472494886825));
#11713=CARTESIAN_POINT('Ctrl Pts',(3.10085066357087,57.7281426935401,-2.29658544858143));
#11714=CARTESIAN_POINT('Ctrl Pts',(3.21310392137964,57.757646036463,-2.40487775337478));
#11715=CARTESIAN_POINT('Ctrl Pts',(3.27253044416714,57.7618592555105,-2.46210260436637));
#11716=CARTESIAN_POINT('Ctrl Pts',(3.33207315476026,57.7556502890384,-2.51964428176192));
#11717=CARTESIAN_POINT('Ctrl Pts',(3.33316746036413,57.755532526842,-2.52070188444734));
#11718=CARTESIAN_POINT('Ctrl Pts',(3.33426151832784,57.7554111397819,-2.52175932309883));
#11719=CARTESIAN_POINT('Origin',(1.15,56.75,-2.));
#11720=CARTESIAN_POINT('',(2.8,55.,-2.));
#11721=CARTESIAN_POINT('Ctrl Pts',(2.8,55.3431808226538,2.5000000000072));
#11722=CARTESIAN_POINT('Ctrl Pts',(2.8,55.418416750227,0.834481782395201));
#11723=CARTESIAN_POINT('Ctrl Pts',(2.8,55.4184191500722,-0.834428656364044));
#11724=CARTESIAN_POINT('Ctrl Pts',(2.8,55.3431808226542,-2.50000000000005));
#11725=CARTESIAN_POINT('Ctrl Pts',(2.8,55.2009701963905,2.493575964374));
#11726=CARTESIAN_POINT('Ctrl Pts',(2.8,55.2760124216453,0.832345787733798));
#11727=CARTESIAN_POINT('Ctrl Pts',(2.8,55.2760148153119,-0.832292798480848));
#11728=CARTESIAN_POINT('Ctrl Pts',(2.8,55.2009701963908,-2.49357596436687));
#11729=CARTESIAN_POINT('Ctrl Pts',(2.86422761419582,55.0599778981397,2.4872069638867));
#11730=CARTESIAN_POINT('Ctrl Pts',(2.86422761419582,55.1348283214914,0.830222758207451));
#11731=CARTESIAN_POINT('Ctrl Pts',(2.86422761419583,55.13483070904,-0.830169904390779));
#11732=CARTESIAN_POINT('Ctrl Pts',(2.86422761419583,55.05997789814,-2.48720696387959));
#11733=CARTESIAN_POINT('Ctrl Pts',(2.97156409628599,54.9665637470306,2.48298719598933));
#11734=CARTESIAN_POINT('Ctrl Pts',(2.97156409628599,55.0412876849674,0.828803032387072));
#11735=CARTESIAN_POINT('Ctrl Pts',(2.971564096286,55.0412900684814,-0.828750267885016));
#11736=CARTESIAN_POINT('Ctrl Pts',(2.971564096286,54.9665637470309,-2.48298719598223));
#11737=CARTESIAN_POINT('',(2.8,55.363504798459,2.00000000000001));
#11738=CARTESIAN_POINT('Ctrl Pts',(2.8,55.3599937696469,2.09491350990412));
#11739=CARTESIAN_POINT('Ctrl Pts',(2.8,55.3611908435143,2.06327665921582));
#11740=CARTESIAN_POINT('Ctrl Pts',(2.8,55.3623607880677,2.03163878205578));
#11741=CARTESIAN_POINT('Ctrl Pts',(2.8,55.3635036032579,1.99999992451711));
#11742=CARTESIAN_POINT('',(2.8,55.363504798459,-1.99999999999998));
#11743=CARTESIAN_POINT('Ctrl Pts',(2.8,55.3635036032579,1.99999992451718));
#11744=CARTESIAN_POINT('Ctrl Pts',(2.8,55.4116430788051,0.667257743744672));
#11745=CARTESIAN_POINT('Ctrl Pts',(2.8,55.4116443040882,-0.66722401754958));
#11746=CARTESIAN_POINT('Ctrl Pts',(2.8,55.363503594285,-2.00000017815421));
#11747=CARTESIAN_POINT('Ctrl Pts',(2.8,55.3599937633195,-2.0949136807012));
#11748=CARTESIAN_POINT('Ctrl Pts',(2.8,55.3611908369837,-2.06327683842182));
#11749=CARTESIAN_POINT('Ctrl Pts',(2.8,55.3623607806224,-2.03163898887636));
#11750=CARTESIAN_POINT('Ctrl Pts',(2.8,55.363503594285,-2.00000017815421));
#11751=CARTESIAN_POINT('Origin',(2.8,55.,0.));
#11752=CARTESIAN_POINT('',(2.8,57.2767060437521,1.99999999999997));
#11753=CARTESIAN_POINT('Ctrl Pts',(2.8,57.2767049572205,2.00000016086605));
#11754=CARTESIAN_POINT('Ctrl Pts',(2.8,57.2767046965456,2.00000762698538));
#11755=CARTESIAN_POINT('Ctrl Pts',(2.8,57.2767044358693,2.00001509310466));
#11756=CARTESIAN_POINT('Ctrl Pts',(2.8,57.2767041751915,2.0000225592239));
#11757=CARTESIAN_POINT('',(2.8,57.2767060437521,-1.99999999999999));
#11758=CARTESIAN_POINT('Ctrl Pts',(2.8,57.2767049649653,-1.99999993439379));
#11759=CARTESIAN_POINT('Ctrl Pts',(2.8,57.3232381590415,-0.667219180437501));
#11760=CARTESIAN_POINT('Ctrl Pts',(2.8,57.3232392879721,0.667187020901882));
#11761=CARTESIAN_POINT('Ctrl Pts',(2.8,57.2767049572205,2.00000016086605));
#11762=CARTESIAN_POINT('Ctrl Pts',(2.8,57.2767049649653,-1.99999993439379));
#11763=CARTESIAN_POINT('Ctrl Pts',(2.8,57.2767047042902,-2.00000740051943));
#11764=CARTESIAN_POINT('Ctrl Pts',(2.8,57.2767044436137,-2.00001486664502));
#11765=CARTESIAN_POINT('Ctrl Pts',(2.8,57.2767041829358,-2.00002233277056));
#11766=CARTESIAN_POINT('Ctrl Pts',(2.8,57.2570611822017,-2.50000000000011));
#11767=CARTESIAN_POINT('Ctrl Pts',(2.8,57.3297855444336,-0.834406696899876));
#11768=CARTESIAN_POINT('Ctrl Pts',(2.8,57.3297877551691,0.834356064814358));
#11769=CARTESIAN_POINT('Ctrl Pts',(2.8,57.2570611822017,2.50000000000002));
#11770=CARTESIAN_POINT('Ctrl Pts',(2.8,57.3935455699524,-2.50595928191804));
#11771=CARTESIAN_POINT('Ctrl Pts',(2.8,57.4664436708706,-0.836386872181238));
#11772=CARTESIAN_POINT('Ctrl Pts',(2.8,57.4664458868875,0.836336119135542));
#11773=CARTESIAN_POINT('Ctrl Pts',(2.8,57.3935455699524,2.50595928191794));
#11774=CARTESIAN_POINT('Ctrl Pts',(2.91867325002229,57.6650888139175,-2.51781560314543));
#11775=CARTESIAN_POINT('Ctrl Pts',(2.91867325002229,57.7383307514702,-0.840368363322168));
#11776=CARTESIAN_POINT('Ctrl Pts',(2.91867325002229,57.7383329779393,0.840317370890855));
#11777=CARTESIAN_POINT('Ctrl Pts',(2.91867325002229,57.6650888139175,2.51781560314534));
#11778=CARTESIAN_POINT('Ctrl Pts',(3.19796820075467,57.7647634644866,-2.5221676711922));
#11779=CARTESIAN_POINT('Ctrl Pts',(3.19796820075467,57.838134288488,-0.841768567659979));
#11780=CARTESIAN_POINT('Ctrl Pts',(3.19796820075467,57.8381365188751,0.841717485495471));
#11781=CARTESIAN_POINT('Ctrl Pts',(3.19796820075467,57.7647634644867,2.52216767119211));
#11782=CARTESIAN_POINT('Ctrl Pts',(3.33426151832784,57.7554111397819,-2.5217593230989));
#11783=CARTESIAN_POINT('Ctrl Pts',(3.33426151832784,57.8287684751718,-0.841669146865329));
#11784=CARTESIAN_POINT('Ctrl Pts',(3.33426151832784,57.8287707051489,0.841618074091848));
#11785=CARTESIAN_POINT('Ctrl Pts',(3.33426151832784,57.7554111397819,2.5217593230988));
#11786=CARTESIAN_POINT('Origin',(11.,20.,0.));
#11787=CARTESIAN_POINT('Origin',(0.3,0.,0.));
#11788=CARTESIAN_POINT('',(0.,0.,0.));
#11789=CARTESIAN_POINT('Origin',(67.15,0.,0.));
#11790=CARTESIAN_POINT('',(67.3,12.6,-1.54305496692567E-15));
#11791=CARTESIAN_POINT('',(67.3,-12.6,-1.54305496692567E-15));
#11792=CARTESIAN_POINT('Origin',(67.3,0.,0.));
#11793=CARTESIAN_POINT('Origin',(67.3,0.,0.));
#11794=CARTESIAN_POINT('',(67.,12.3,1.50631556295124E-15));
#11795=CARTESIAN_POINT('',(67.15,12.45,1.52468526493846E-15));
#11796=CARTESIAN_POINT('Origin',(67.,0.,0.));
#11797=CARTESIAN_POINT('Origin',(67.6,0.,0.));
#11798=CARTESIAN_POINT('',(67.9,12.6,1.54305496692567E-15));
#11799=CARTESIAN_POINT('',(67.9,-12.6,-1.54305496692567E-15));
#11800=CARTESIAN_POINT('Origin',(67.9,0.,0.));
#11801=CARTESIAN_POINT('Origin',(67.9,0.,0.));
#11802=CARTESIAN_POINT('',(67.6,-12.6,-1.54305496692567E-15));
#11803=CARTESIAN_POINT('Origin',(67.,12.6,0.));
#11804=CARTESIAN_POINT('',(67.,-1.29812560709619E-15,10.6));
#11805=CARTESIAN_POINT('Origin',(67.,0.,0.));
#11806=CARTESIAN_POINT('Origin',(68.05,0.,0.));
#11807=CARTESIAN_POINT('',(68.2,12.3,-1.50631556295124E-15));
#11808=CARTESIAN_POINT('Origin',(68.2,0.,0.));
#11809=CARTESIAN_POINT('',(68.05,12.45,1.52468526493846E-15));
#11810=CARTESIAN_POINT('Origin',(68.2,10.5,0.));
#11811=CARTESIAN_POINT('',(68.2,-11.,-1.34711147906209E-15));
#11812=CARTESIAN_POINT('Origin',(68.2,0.,0.));
#11813=CARTESIAN_POINT('Origin',(67.6,0.,0.));
#11814=CARTESIAN_POINT('',(67.,10.24,-2.32215417231501));
#11815=CARTESIAN_POINT('',(68.2,10.24,-2.32215417231501));
#11816=CARTESIAN_POINT('',(67.6,10.24,-2.32215417231501));
#11817=CARTESIAN_POINT('',(67.,10.1980390271856,-2.5));
#11818=CARTESIAN_POINT('Origin',(67.,0.,0.));
#11819=CARTESIAN_POINT('',(68.2,10.1980390271856,-2.5));
#11820=CARTESIAN_POINT('',(67.6,10.1980390271856,-2.5));
#11821=CARTESIAN_POINT('Origin',(68.2,0.,0.));
#11822=CARTESIAN_POINT('Origin',(67.6,0.,0.));
#11823=CARTESIAN_POINT('',(68.2,10.24,2.32215417231501));
#11824=CARTESIAN_POINT('',(67.,10.24,2.32215417231501));
#11825=CARTESIAN_POINT('',(67.6,10.24,2.32215417231501));
#11826=CARTESIAN_POINT('',(68.2,10.1980390271856,2.5));
#11827=CARTESIAN_POINT('Origin',(68.2,0.,0.));
#11828=CARTESIAN_POINT('',(67.,10.1980390271856,2.5));
#11829=CARTESIAN_POINT('',(67.6,10.1980390271856,2.5));
#11830=CARTESIAN_POINT('Origin',(67.,0.,0.));
#11831=CARTESIAN_POINT('Origin',(68.2,10.5,0.));
#11832=CARTESIAN_POINT('',(68.2,10.24,-2.5));
#11833=CARTESIAN_POINT('',(68.2,10.24,0.));
#11834=CARTESIAN_POINT('',(68.2,9.56,-2.5));
#11835=CARTESIAN_POINT('Origin',(68.2,10.5,0.));
#11836=CARTESIAN_POINT('',(68.2,10.24,2.5));
#11837=CARTESIAN_POINT('',(68.2,10.24,0.));
#11838=CARTESIAN_POINT('',(68.2,9.56,2.5));
#11839=CARTESIAN_POINT('Origin',(67.,12.6,0.));
#11840=CARTESIAN_POINT('',(67.,10.24,-2.5));
#11841=CARTESIAN_POINT('',(67.,10.24,0.));
#11842=CARTESIAN_POINT('',(67.,10.61,-2.5));
#11843=CARTESIAN_POINT('Origin',(67.,12.6,0.));
#11844=CARTESIAN_POINT('',(67.,10.24,2.5));
#11845=CARTESIAN_POINT('',(67.,10.24,0.));
#11846=CARTESIAN_POINT('',(67.,10.61,2.5));
#11847=CARTESIAN_POINT('Origin',(58.5,8.62,2.5));
#11848=CARTESIAN_POINT('',(69.,10.24,2.5));
#11849=CARTESIAN_POINT('',(69.,10.24,2.5));
#11850=CARTESIAN_POINT('',(69.,7.9669630349337,2.5));
#11851=CARTESIAN_POINT('',(69.,7.,2.5));
#11852=CARTESIAN_POINT('',(69.0218379181362,7.83022988168291,2.5));
#11853=CARTESIAN_POINT('Ctrl Pts',(69.0218379181362,7.83022988168291,2.5));
#11854=CARTESIAN_POINT('Ctrl Pts',(69.0075947074924,7.87360329207051,2.5));
#11855=CARTESIAN_POINT('Ctrl Pts',(69.,7.92356314245502,2.5));
#11856=CARTESIAN_POINT('Ctrl Pts',(69.,7.96696303493369,2.5));
#11857=CARTESIAN_POINT('',(49.1,7.83022988168291,2.5));
#11858=CARTESIAN_POINT('',(59.6,7.83022988168291,2.5));
#11859=CARTESIAN_POINT('',(49.1000000000041,9.91907544765526,2.5));
#11860=CARTESIAN_POINT('',(49.1,9.56,2.5));
#11861=CARTESIAN_POINT('',(49.4711020394073,10.3051416724427,2.5));
#11862=CARTESIAN_POINT('Ctrl Pts',(49.471102006026,10.3051417027149,2.5));
#11863=CARTESIAN_POINT('Ctrl Pts',(49.3473096739212,10.176541099224,2.5));
#11864=CARTESIAN_POINT('Ctrl Pts',(49.2236056134068,10.0478555238674,2.5));
#11865=CARTESIAN_POINT('Ctrl Pts',(49.1000000000083,9.91907544765526,2.5));
#11866=CARTESIAN_POINT('',(49.2908747206533,10.7048947780346,2.50000000015575));
#11867=CARTESIAN_POINT('Ctrl Pts',(49.4711018427219,10.3051416733467,2.49999916236061));
#11868=CARTESIAN_POINT('Ctrl Pts',(49.4521138045415,10.3172467342247,2.4999991258175));
#11869=CARTESIAN_POINT('Ctrl Pts',(49.434143505605,10.330934192123,2.49999638873673));
#11870=CARTESIAN_POINT('Ctrl Pts',(49.4173733976671,10.3460508501851,2.49999630498322));
#11871=CARTESIAN_POINT('Ctrl Pts',(49.4122331919494,10.3506842569879,2.49999627931193));
#11872=CARTESIAN_POINT('Ctrl Pts',(49.407206024932,10.3554521608227,2.49999644341522));
#11873=CARTESIAN_POINT('Ctrl Pts',(49.4022979734507,10.3603506775391,2.49999677600973));
#11874=CARTESIAN_POINT('Ctrl Pts',(49.3864116942846,10.3762060947765,2.49999785254475));
#11875=CARTESIAN_POINT('Ctrl Pts',(49.3718997498427,10.39329834119,2.50000118698146));
#11876=CARTESIAN_POINT('Ctrl Pts',(49.3589269316826,10.4114566220581,2.50000300029283));
#11877=CARTESIAN_POINT('Ctrl Pts',(49.350246313729,10.4236070350959,2.5000042136501));
#11878=CARTESIAN_POINT('Ctrl Pts',(49.3422554681063,10.4362356041593,2.50000459747335));
#11879=CARTESIAN_POINT('Ctrl Pts',(49.3350146148726,10.4492980430834,2.50000044385569));
#11880=CARTESIAN_POINT('Ctrl Pts',(49.3281858085234,10.4616171528597,2.49999652660315));
#11881=CARTESIAN_POINT('Ctrl Pts',(49.322024170055,10.4743223572284,2.49998855549731));
#11882=CARTESIAN_POINT('Ctrl Pts',(49.3165487906394,10.4873606414204,2.49998021758341));
#11883=CARTESIAN_POINT('Ctrl Pts',(49.3078883482859,10.5079833782326,2.49996702945212));
#11884=CARTESIAN_POINT('Ctrl Pts',(49.3010202713955,10.5292527079667,2.49995372503714));
#11885=CARTESIAN_POINT('Ctrl Pts',(49.295964487035,10.5509344138267,2.49994954600057));
#11886=CARTESIAN_POINT('Ctrl Pts',(49.2909278369453,10.5725340624628,2.49994538278011));
#11887=CARTESIAN_POINT('Ctrl Pts',(49.2876895556668,10.5945443716744,2.49995033506508));
#11888=CARTESIAN_POINT('Ctrl Pts',(49.2863171078659,10.616744070017,2.49996099739857));
#11889=CARTESIAN_POINT('Ctrl Pts',(49.2859316121374,10.6229795631829,2.49996399225492));
#11890=CARTESIAN_POINT('Ctrl Pts',(49.2856936230256,10.6292299902788,2.49996735822794));
#11891=CARTESIAN_POINT('Ctrl Pts',(49.2856053589302,10.6354903616755,2.49997082976491));
#11892=CARTESIAN_POINT('Ctrl Pts',(49.2852767142312,10.6588003821638,2.49998375577085));
#11893=CARTESIAN_POINT('Ctrl Pts',(49.2870227193347,10.6820201214405,2.49999973692703));
#11894=CARTESIAN_POINT('Ctrl Pts',(49.2908747205558,10.7048947773733,2.49999999901159));
#11895=CARTESIAN_POINT('',(49.3656854249492,10.7121426428143,2.5));
#11896=CARTESIAN_POINT('Ctrl Pts',(49.3656854249492,10.7121426428143,2.5));
#11897=CARTESIAN_POINT('Ctrl Pts',(49.3420008434391,10.7121426428143,2.5));
#11898=CARTESIAN_POINT('Ctrl Pts',(49.316211839325,10.7098484152381,2.5));
#11899=CARTESIAN_POINT('Ctrl Pts',(49.2908747205092,10.7048947787715,2.5));
#11900=CARTESIAN_POINT('',(50.0760927660041,10.7121954410373,2.49981008259284));
#11901=CARTESIAN_POINT('',(58.1,10.7121426428143,2.5));
#11902=CARTESIAN_POINT('',(50.4873080527574,10.24,2.5000000001691));
#11903=CARTESIAN_POINT('Ctrl Pts',(50.0760927937211,10.7121954053708,2.49981021088675));
#11904=CARTESIAN_POINT('Ctrl Pts',(50.0724347185981,10.6931913800779,2.49980703933385));
#11905=CARTESIAN_POINT('Ctrl Pts',(50.0702493871277,10.6739403201419,2.4997968810974));
#11906=CARTESIAN_POINT('Ctrl Pts',(50.069525629523,10.654595400641,2.49979096643753));
#11907=CARTESIAN_POINT('Ctrl Pts',(50.0687949509244,10.6350654936968,2.49978499521822));
#11908=CARTESIAN_POINT('Ctrl Pts',(50.0695567922128,10.6155130900928,2.49978334870012));
#11909=CARTESIAN_POINT('Ctrl Pts',(50.0717964790934,10.5960964549971,2.49978810400288));
#11910=CARTESIAN_POINT('Ctrl Pts',(50.074056422491,10.576504209014,2.49979290231427));
#11911=CARTESIAN_POINT('Ctrl Pts',(50.0778126805385,10.5571242161645,2.49980421827627));
#11912=CARTESIAN_POINT('Ctrl Pts',(50.0830446502572,10.5381168834534,2.49981480884476));
#11913=CARTESIAN_POINT('Ctrl Pts',(50.085301988002,10.5299161537353,2.49981937815446));
#11914=CARTESIAN_POINT('Ctrl Pts',(50.0878292904794,10.5218034036804,2.49982375513529));
#11915=CARTESIAN_POINT('Ctrl Pts',(50.0906226140567,10.5137908789098,2.49982683752301));
#11916=CARTESIAN_POINT('Ctrl Pts',(50.0979560533961,10.4927552334733,2.49983492985557));
#11917=CARTESIAN_POINT('Ctrl Pts',(50.1071191248528,10.4724097745267,2.49983508259961));
#11918=CARTESIAN_POINT('Ctrl Pts',(50.1179434009193,10.4529284325733,2.49984014939377));
#11919=CARTESIAN_POINT('Ctrl Pts',(50.1223596888886,10.4449800750514,2.49984221663798));
#11920=CARTESIAN_POINT('Ctrl Pts',(50.1270531075935,10.4371756491499,2.49984495292356));
#11921=CARTESIAN_POINT('Ctrl Pts',(50.1320145050724,10.4295276315651,2.49984866910354));
#11922=CARTESIAN_POINT('Ctrl Pts',(50.1445994971712,10.4101278069619,2.4998580954992));
#11923=CARTESIAN_POINT('Ctrl Pts',(50.1588049548903,10.3918873519457,2.49987278486773));
#11924=CARTESIAN_POINT('Ctrl Pts',(50.1744316650975,10.374977827846,2.49989012485888));
#11925=CARTESIAN_POINT('Ctrl Pts',(50.1841474977131,10.3644644118048,2.49990090591576));
#11926=CARTESIAN_POINT('Ctrl Pts',(50.1944138546499,10.3544654862454,2.49991239300784));
#11927=CARTESIAN_POINT('Ctrl Pts',(50.2051921016056,10.345025159572,2.49992124592571));
#11928=CARTESIAN_POINT('Ctrl Pts',(50.2160584446486,10.3355076723135,2.49993017120298));
#11929=CARTESIAN_POINT('Ctrl Pts',(50.2274450835419,10.326557775575,2.49993643693284));
#11930=CARTESIAN_POINT('Ctrl Pts',(50.2392963798676,10.3182015287255,2.49994151742415));
#11931=CARTESIAN_POINT('Ctrl Pts',(50.2582120637921,10.3048642430937,2.4999496263234));
#11932=CARTESIAN_POINT('Ctrl Pts',(50.2781856685745,10.2931249989061,2.49995479742236));
#11933=CARTESIAN_POINT('Ctrl Pts',(50.2989721259798,10.2830646910121,2.49996241168663));
#11934=CARTESIAN_POINT('Ctrl Pts',(50.3116765962231,10.2769159336849,2.49996706544709));
#11935=CARTESIAN_POINT('Ctrl Pts',(50.3246856114912,10.2713948751988,2.49997229683092));
#11936=CARTESIAN_POINT('Ctrl Pts',(50.3379495491142,10.2665266123185,2.49997672454703));
#11937=CARTESIAN_POINT('Ctrl Pts',(50.3446721543995,10.2640592145743,2.499978968661));
#11938=CARTESIAN_POINT('Ctrl Pts',(50.3514603069851,10.2617595967717,2.49998097829715));
#11939=CARTESIAN_POINT('Ctrl Pts',(50.3583070707371,10.2596289619541,2.49998265182534));
#11940=CARTESIAN_POINT('Ctrl Pts',(50.3807108950684,10.2526571472551,2.49998812790615));
#11941=CARTESIAN_POINT('Ctrl Pts',(50.4036318885686,10.2475250346903,2.49999069009023));
#11942=CARTESIAN_POINT('Ctrl Pts',(50.4268185719221,10.244255753949,2.49999402764095));
#11943=CARTESIAN_POINT('Ctrl Pts',(50.4468344518825,10.2414335507957,2.49999690877808));
#11944=CARTESIAN_POINT('Ctrl Pts',(50.4670493379255,10.24,2.49999999999998));
#11945=CARTESIAN_POINT('Ctrl Pts',(50.4873080526582,10.24,2.5));
#11946=CARTESIAN_POINT('',(69.,10.24,2.5));
#11947=CARTESIAN_POINT('Ctrl Pts',(50.10596357807,10.6854183957887,2.61186402918292));
#11948=CARTESIAN_POINT('Ctrl Pts',(50.0460788562875,10.7408164456412,2.38522461213428));
#11949=CARTESIAN_POINT('Ctrl Pts',(49.9164083980935,10.8391161748358,1.92156092596857));
#11950=CARTESIAN_POINT('Ctrl Pts',(49.7576509378753,10.9271110146993,1.30914434152331));
#11951=CARTESIAN_POINT('Ctrl Pts',(49.666672528926,10.967422685746,0.865348982805604));
#11952=CARTESIAN_POINT('Ctrl Pts',(49.6243567523392,10.9841733422946,0.604311373359717));
#11953=CARTESIAN_POINT('Ctrl Pts',(49.5997258546835,10.9933200965768,0.404693900681247));
#11954=CARTESIAN_POINT('Ctrl Pts',(49.5716547215071,11.0027241723402,0.0691641331704865));
#11955=CARTESIAN_POINT('Ctrl Pts',(49.5900774295882,10.9974150814697,-0.476621441399214));
#11956=CARTESIAN_POINT('Ctrl Pts',(49.7280572779163,10.9444131408942,-1.18870751171882));
#11957=CARTESIAN_POINT('Ctrl Pts',(49.915841181391,10.8391437000355,-1.92085485622915));
#11958=CARTESIAN_POINT('Ctrl Pts',(50.0460661791746,10.7408281729562,-2.38517663440393));
#11959=CARTESIAN_POINT('Ctrl Pts',(50.1059635780249,10.6854183958305,-2.61186402901213));
#11960=CARTESIAN_POINT('Ctrl Pts',(50.0989714172686,10.6216586600213,2.6139151177149));
#11961=CARTESIAN_POINT('Ctrl Pts',(50.0300443077418,10.672816415315,2.39024416325827));
#11962=CARTESIAN_POINT('Ctrl Pts',(49.8808171508488,10.7675718810144,1.93499669767664));
#11963=CARTESIAN_POINT('Ctrl Pts',(49.6975309544909,10.862958211197,1.33199623935741));
#11964=CARTESIAN_POINT('Ctrl Pts',(49.5912646760291,10.912041457587,0.888629458300868));
#11965=CARTESIAN_POINT('Ctrl Pts',(49.5411396412093,10.9338315137794,0.624351882943105));
#11966=CARTESIAN_POINT('Ctrl Pts',(49.5117069919845,10.9462019721493,0.420209333159837));
#11967=CARTESIAN_POINT('Ctrl Pts',(49.4773242232257,10.9598077704949,0.0728776092390634));
#11968=CARTESIAN_POINT('Ctrl Pts',(49.5006330977212,10.9512789811939,-0.498940433437269));
#11969=CARTESIAN_POINT('Ctrl Pts',(49.6638979089462,10.8811822008758,-1.21335763832631));
#11970=CARTESIAN_POINT('Ctrl Pts',(49.8800144260071,10.7677624922463,-1.93434775525291));
#11971=CARTESIAN_POINT('Ctrl Pts',(50.0300297164284,10.6728272449952,-2.39019681392804));
#11972=CARTESIAN_POINT('Ctrl Pts',(50.0989714172167,10.6216586600599,-2.61391511754634));
#11973=CARTESIAN_POINT('Ctrl Pts',(50.1150024369948,10.4905936402599,2.60921255985761));
#11974=CARTESIAN_POINT('Ctrl Pts',(50.0322851458687,10.5282606753826,2.3888654393634));
#11975=CARTESIAN_POINT('Ctrl Pts',(49.8507006451456,10.602551600071,1.94594986862127));
#11976=CARTESIAN_POINT('Ctrl Pts',(49.6201589477057,10.6899004066302,1.36161040345567));
#11977=CARTESIAN_POINT('Ctrl Pts',(49.4811686636315,10.7412549980383,0.922685634553976));
#11978=CARTESIAN_POINT('Ctrl Pts',(49.4137309602737,10.7655984033572,0.655012650144937));
#11979=CARTESIAN_POINT('Ctrl Pts',(49.3734928710052,10.7799234763981,0.444625304668301));
#11980=CARTESIAN_POINT('Ctrl Pts',(49.3247495826024,10.796604039827,0.0790162780648425));
#11981=CARTESIAN_POINT('Ctrl Pts',(49.3592937415449,10.7853242476646,-0.535131696197622));
#11982=CARTESIAN_POINT('Ctrl Pts',(49.5791556288816,10.7058491105962,-1.24644054242593));
#11983=CARTESIAN_POINT('Ctrl Pts',(49.8493254724924,10.60293912814,-1.94543141854448));
#11984=CARTESIAN_POINT('Ctrl Pts',(50.0322676352843,10.5282686491883,-2.38881879366335));
#11985=CARTESIAN_POINT('Ctrl Pts',(50.1150024369325,10.4905936402883,-2.60921255969157));
#11986=CARTESIAN_POINT('Ctrl Pts',(50.2146309334458,10.3415545946635,2.57998742154472));
#11987=CARTESIAN_POINT('Ctrl Pts',(50.1280147436699,10.3579163649357,2.35632872799266));
#11988=CARTESIAN_POINT('Ctrl Pts',(49.9329267878874,10.3913302277352,1.91381270831632));
#11989=CARTESIAN_POINT('Ctrl Pts',(49.6753913671128,10.4341807413213,1.34149299628219));
#11990=CARTESIAN_POINT('Ctrl Pts',(49.515517131939,10.4611489433235,0.912449575184171));
#11991=CARTESIAN_POINT('Ctrl Pts',(49.4368991664712,10.4743372237122,0.649532628539433));
#11992=CARTESIAN_POINT('Ctrl Pts',(49.3896820250642,10.4822188796987,0.441974264929375));
#11993=CARTESIAN_POINT('Ctrl Pts',(49.331903164895,10.4916293139201,0.0790634742199547));
#11994=CARTESIAN_POINT('Ctrl Pts',(49.3733374267131,10.4850633550494,-0.53401775304525));
#11995=CARTESIAN_POINT('Ctrl Pts',(49.6302127509665,10.441780875437,-1.22860722352935));
#11996=CARTESIAN_POINT('Ctrl Pts',(49.931195998432,10.3915871925538,-1.91338712054486));
#11997=CARTESIAN_POINT('Ctrl Pts',(50.1279964077188,10.35791982859,-2.35628138126123));
#11998=CARTESIAN_POINT('Ctrl Pts',(50.2146309333805,10.3415545946759,-2.57998742137617));
#11999=CARTESIAN_POINT('Ctrl Pts',(50.3487993253124,10.2576120585743,2.54063031038476));
#12000=CARTESIAN_POINT('Ctrl Pts',(50.268468199078,10.2605598936513,2.30911926875332));
#12001=CARTESIAN_POINT('Ctrl Pts',(50.0829097045463,10.2667082145781,1.85595146364309));
#12002=CARTESIAN_POINT('Ctrl Pts',(49.834412994289,10.2748729796263,1.28196538532196));
#12003=CARTESIAN_POINT('Ctrl Pts',(49.680835270301,10.280139448227,0.861728214240658));
#12004=CARTESIAN_POINT('Ctrl Pts',(49.6060998009801,10.2827398747948,0.608877935796896));
#12005=CARTESIAN_POINT('Ctrl Pts',(49.5614948221163,10.2843033157519,0.411842146135796));
#12006=CARTESIAN_POINT('Ctrl Pts',(49.5079282298224,10.286183251424,0.0724642239699666));
#12007=CARTESIAN_POINT('Ctrl Pts',(49.5454900245608,10.2848624181149,-0.49295565087574));
#12008=CARTESIAN_POINT('Ctrl Pts',(49.7901458075476,10.2763008155086,-1.1689093490474));
#12009=CARTESIAN_POINT('Ctrl Pts',(50.0814081572479,10.2667616581884,-1.85544105748007));
#12010=CARTESIAN_POINT('Ctrl Pts',(50.2684511936231,10.2605605176842,-2.30907025974476));
#12011=CARTESIAN_POINT('Ctrl Pts',(50.3487993252519,10.2576120585765,-2.5406303102103));
#12012=CARTESIAN_POINT('Ctrl Pts',(50.4411230608376,10.24,2.51354795908566));
#12013=CARTESIAN_POINT('Ctrl Pts',(50.3672699512713,10.2399851855682,2.27600839076339));
#12014=CARTESIAN_POINT('Ctrl Pts',(50.1936849991744,10.2399659210815,1.81340446242885));
#12015=CARTESIAN_POINT('Ctrl Pts',(49.9605600409879,10.2399459207391,1.2347012119753));
#12016=CARTESIAN_POINT('Ctrl Pts',(49.8184924102703,10.2399466460418,0.819505327343819));
#12017=CARTESIAN_POINT('Ctrl Pts',(49.7504193447077,10.2399497034154,0.574248649565897));
#12018=CARTESIAN_POINT('Ctrl Pts',(49.7101658107336,10.2399531561777,0.385760776646267));
#12019=CARTESIAN_POINT('Ctrl Pts',(49.6629992153512,10.2399589729157,0.0665545800454013));
#12020=CARTESIAN_POINT('Ctrl Pts',(49.6950815292353,10.239953993875,-0.456754223466842));
#12021=CARTESIAN_POINT('Ctrl Pts',(49.9181644279458,10.239937833965,-1.12092692435959));
#12022=CARTESIAN_POINT('Ctrl Pts',(50.1924973076596,10.2399668152967,-1.81280733835446));
#12023=CARTESIAN_POINT('Ctrl Pts',(50.3672543171596,10.2399851824321,-2.27595810556525));
#12024=CARTESIAN_POINT('Ctrl Pts',(50.441123060782,10.24,-2.51354795890666));
#12025=CARTESIAN_POINT('Ctrl Pts',(50.4873080527118,10.24,2.5000000001825));
#12026=CARTESIAN_POINT('Ctrl Pts',(50.4167383525177,10.24,2.25942789236011));
#12027=CARTESIAN_POINT('Ctrl Pts',(50.2491743046301,10.24,1.79205452172678));
#12028=CARTESIAN_POINT('Ctrl Pts',(50.0239314790447,10.24,1.21089457224777));
#12029=CARTESIAN_POINT('Ctrl Pts',(49.8878049235054,10.24,0.798190480225308));
#12030=CARTESIAN_POINT('Ctrl Pts',(49.8231790425819,10.24,0.556751291784615));
#12031=CARTESIAN_POINT('Ctrl Pts',(49.7851714883371,10.24,0.372575689154406));
#12032=CARTESIAN_POINT('Ctrl Pts',(49.7413090623653,10.24,0.0635723530955229));
#12033=CARTESIAN_POINT('Ctrl Pts',(49.7705555891009,10.24,-0.43840113636878));
#12034=CARTESIAN_POINT('Ctrl Pts',(49.9825087104814,10.24,-1.09672361261615));
#12035=CARTESIAN_POINT('Ctrl Pts',(50.2481483914462,10.24,-1.79140201558762));
#12036=CARTESIAN_POINT('Ctrl Pts',(50.4167234134771,10.24,-2.25937696519828));
#12037=CARTESIAN_POINT('Ctrl Pts',(50.4873080526586,10.24,-2.50000000000121));
#12038=CARTESIAN_POINT('',(50.4873080526589,10.24,-2.50000000000112));
#12039=CARTESIAN_POINT('',(50.0760766664832,10.712193812233,-2.49979592332684));
#12040=CARTESIAN_POINT('Ctrl Pts',(50.4873080526582,10.24,-2.5));
#12041=CARTESIAN_POINT('Ctrl Pts',(50.4641571594583,10.24,-2.5));
#12042=CARTESIAN_POINT('Ctrl Pts',(50.4410809471426,10.2418709746727,-2.49999428716151));
#12043=CARTESIAN_POINT('Ctrl Pts',(50.4183088007534,10.2455410414974,-2.49998945021977));
#12044=CARTESIAN_POINT('Ctrl Pts',(50.3953275608783,10.2492448068172,-2.49998456886531));
#12045=CARTESIAN_POINT('Ctrl Pts',(50.3726546190859,10.2547813030666,-2.49998094173844));
#12046=CARTESIAN_POINT('Ctrl Pts',(50.3505360224068,10.2621263928632,-2.4999763370001));
#12047=CARTESIAN_POINT('Ctrl Pts',(50.3463173584445,10.2635273165327,-2.49997545874168));
#12048=CARTESIAN_POINT('Ctrl Pts',(50.3421189250459,10.2649941656051,-2.49997450960908));
#12049=CARTESIAN_POINT('Ctrl Pts',(50.3379425354016,10.2665269556365,-2.499973420438));
#12050=CARTESIAN_POINT('Ctrl Pts',(50.3319465679701,10.2687275546922,-2.49997185673468));
#12051=CARTESIAN_POINT('Ctrl Pts',(50.3259960277548,10.2710640639799,-2.49997000822049));
#12052=CARTESIAN_POINT('Ctrl Pts',(50.3200958828164,10.2735348019973,-2.49996776320823));
#12053=CARTESIAN_POINT('Ctrl Pts',(50.2989516264854,10.2823891468498,-2.49995971779324));
#12054=CARTESIAN_POINT('Ctrl Pts',(50.2785893166508,10.2929069318771,-2.49994874716809));
#12055=CARTESIAN_POINT('Ctrl Pts',(50.2592178604724,10.3049773058068,-2.4999397329224));
#12056=CARTESIAN_POINT('Ctrl Pts',(50.2401649112326,10.316849217741,-2.49993086688961));
#12057=CARTESIAN_POINT('Ctrl Pts',(50.222069498692,10.3302239956641,-2.49992413432698));
#12058=CARTESIAN_POINT('Ctrl Pts',(50.2051646417189,10.3450289994691,-2.49991117822164));
#12059=CARTESIAN_POINT('Ctrl Pts',(50.197210595605,10.3519950260477,-2.4999050821358));
#12060=CARTESIAN_POINT('Ctrl Pts',(50.1895207594136,10.3592781180278,-2.49989737920897));
#12061=CARTESIAN_POINT('Ctrl Pts',(50.1821140026648,10.3668627737153,-2.49988876547526));
#12062=CARTESIAN_POINT('Ctrl Pts',(50.165999922145,10.3833638897375,-2.49987002550536));
#12063=CARTESIAN_POINT('Ctrl Pts',(50.151356493375,10.4011543565194,-2.49985067555682));
#12064=CARTESIAN_POINT('Ctrl Pts',(50.1383299981319,10.4200373670364,-2.49983801584716));
#12065=CARTESIAN_POINT('Ctrl Pts',(50.1257967192861,10.4382054185223,-2.49982583546645));
#12066=CARTESIAN_POINT('Ctrl Pts',(50.1147597288176,10.4573861991229,-2.49981998122588));
#12067=CARTESIAN_POINT('Ctrl Pts',(50.105392687849,10.4774188980176,-2.49981541575245));
#12068=CARTESIAN_POINT('Ctrl Pts',(50.1021188952813,10.4844203514085,-2.49981382011376));
#12069=CARTESIAN_POINT('Ctrl Pts',(50.0990495236464,10.4915259093987,-2.4998122667488));
#12070=CARTESIAN_POINT('Ctrl Pts',(50.096193480471,10.4987286999449,-2.49981014733828));
#12071=CARTESIAN_POINT('Ctrl Pts',(50.0942154074463,10.5037172959875,-2.49980867945124));
#12072=CARTESIAN_POINT('Ctrl Pts',(50.0923436965187,10.5087424589632,-2.49980700430729));
#12073=CARTESIAN_POINT('Ctrl Pts',(50.090580189988,10.5138015741308,-2.49980482970845));
#12074=CARTESIAN_POINT('Ctrl Pts',(50.0830548124857,10.535390238988,-2.49979555008463));
#12075=CARTESIAN_POINT('Ctrl Pts',(50.0774959148627,10.557596686582,-2.49977795996577));
#12076=CARTESIAN_POINT('Ctrl Pts',(50.0739341814136,10.5801728194331,-2.49976761437599));
#12077=CARTESIAN_POINT('Ctrl Pts',(50.0726394342436,10.5883796054086,-2.49976385358836));
#12078=CARTESIAN_POINT('Ctrl Pts',(50.0716090801445,10.5966352786126,-2.49976095198664));
#12079=CARTESIAN_POINT('Ctrl Pts',(50.0708462864984,10.604927788451,-2.4997593080838));
#12080=CARTESIAN_POINT('Ctrl Pts',(50.0688248378512,10.6269034340006,-2.49975495164327));
#12081=CARTESIAN_POINT('Ctrl Pts',(50.0686944970557,10.6489677176883,-2.49976023269914));
#12082=CARTESIAN_POINT('Ctrl Pts',(50.0704571109796,10.6708939952819,-2.49976785447707));
#12083=CARTESIAN_POINT('Ctrl Pts',(50.0715698352885,10.6847358818991,-2.49977266604554));
#12084=CARTESIAN_POINT('Ctrl Pts',(50.0734379057857,10.6985230156386,-2.49977821610713));
#12085=CARTESIAN_POINT('Ctrl Pts',(50.0760723344211,10.7121976923269,-2.49978044852387));
#12086=CARTESIAN_POINT('Ctrl Pts',(50.4873080526586,10.24,-2.50000000000121));
#12087=CARTESIAN_POINT('Ctrl Pts',(50.4167234134771,10.24,-2.25937696519828));
#12088=CARTESIAN_POINT('Ctrl Pts',(50.2481483914462,10.24,-1.79140201558762));
#12089=CARTESIAN_POINT('Ctrl Pts',(49.9825087104814,10.24,-1.09672361261615));
#12090=CARTESIAN_POINT('Ctrl Pts',(49.7705555891009,10.24,-0.43840113636878));
#12091=CARTESIAN_POINT('Ctrl Pts',(49.7413090623653,10.24,0.0635723530955229));
#12092=CARTESIAN_POINT('Ctrl Pts',(49.7851714883371,10.24,0.372575689154406));
#12093=CARTESIAN_POINT('Ctrl Pts',(49.8231790425819,10.24,0.556751291784615));
#12094=CARTESIAN_POINT('Ctrl Pts',(49.8878049235054,10.24,0.798190480225308));
#12095=CARTESIAN_POINT('Ctrl Pts',(50.0239314790447,10.24,1.21089457224777));
#12096=CARTESIAN_POINT('Ctrl Pts',(50.2491743046301,10.24,1.79205452172678));
#12097=CARTESIAN_POINT('Ctrl Pts',(50.4167383525177,10.24,2.25942789236011));
#12098=CARTESIAN_POINT('Ctrl Pts',(50.4873080527118,10.24,2.5000000001825));
#12099=CARTESIAN_POINT('Ctrl Pts',(50.0760927937211,10.7121954053708,2.49981021088675));
#12100=CARTESIAN_POINT('Ctrl Pts',(50.0248077296735,10.7567670989664,2.30892405297712));
#12101=CARTESIAN_POINT('Ctrl Pts',(49.9707084492665,10.796890351521,2.11425277588037));
#12102=CARTESIAN_POINT('Ctrl Pts',(49.9170745205984,10.8321402105099,1.91499353062095));
#12103=CARTESIAN_POINT('Ctrl Pts',(49.8529054140062,10.8743141107812,1.67659429219047));
#12104=CARTESIAN_POINT('Ctrl Pts',(49.7894024299189,10.9095120467266,1.43162765841236));
#12105=CARTESIAN_POINT('Ctrl Pts',(49.733576327052,10.9366015191072,1.18090721526053));
#12106=CARTESIAN_POINT('Ctrl Pts',(49.7056632756186,10.9501462552974,1.05554699368462));
#12107=CARTESIAN_POINT('Ctrl Pts',(49.6796694444902,10.9616638755964,0.928748319765275));
#12108=CARTESIAN_POINT('Ctrl Pts',(49.6568995752518,10.9710866345457,0.799469558643532));
#12109=CARTESIAN_POINT('Ctrl Pts',(49.6455146406326,10.9757980140203,0.73483017808266));
#12110=CARTESIAN_POINT('Ctrl Pts',(49.6349356964859,10.9799856781574,0.669570775721189));
#12111=CARTESIAN_POINT('Ctrl Pts',(49.6255410748033,10.983603969273,0.603671495760708));
#12112=CARTESIAN_POINT('Ctrl Pts',(49.6161464531206,10.9872222603887,0.537772215800227));
#12113=CARTESIAN_POINT('Ctrl Pts',(49.6079361539021,10.9902711784827,0.471233058240737));
#12114=CARTESIAN_POINT('Ctrl Pts',(49.6010238909752,10.9927360451061,0.404410502709916));
#12115=CARTESIAN_POINT('Ctrl Pts',(49.5941116280482,10.9952009117295,0.337587947179095));
#12116=CARTESIAN_POINT('Ctrl Pts',(49.5884974014129,10.9970817268822,0.270481993676943));
#12117=CARTESIAN_POINT('Ctrl Pts',(49.584862441064,10.998326429157,0.203096729345026));
#12118=CARTESIAN_POINT('Ctrl Pts',(49.5739575600172,11.0020605359813,0.000940936349274404));
#12119=CARTESIAN_POINT('Ctrl Pts',(49.5808660755476,11.0000696269049,-0.203728654114363));
#12120=CARTESIAN_POINT('Ctrl Pts',(49.6009413134475,10.9927369325602,-0.403913545195877));
#12121=CARTESIAN_POINT('Ctrl Pts',(49.6277082973141,10.9829600067673,-0.670826733304562));
#12122=CARTESIAN_POINT('Ctrl Pts',(49.6778827876152,10.9636865738307,-0.929767122511692));
#12123=CARTESIAN_POINT('Ctrl Pts',(49.7342673500115,10.9365049505527,-1.18126187453365));
#12124=CARTESIAN_POINT('Ctrl Pts',(49.7906519124079,10.9093233272746,-1.4327566265556));
#12125=CARTESIAN_POINT('Ctrl Pts',(49.8532465468994,10.8742335136551,-1.67680574139238));
#12126=CARTESIAN_POINT('Ctrl Pts',(49.9171001135911,10.8321097250754,-1.91491074335446));
#12127=CARTESIAN_POINT('Ctrl Pts',(49.9704714803631,10.7969009765812,-2.1139284341172));
#12128=CARTESIAN_POINT('Ctrl Pts',(50.0247223731089,10.7567780923798,-2.30879339793801));
#12129=CARTESIAN_POINT('Ctrl Pts',(50.0760723344211,10.7121976923269,-2.49978044852387));
#12130=CARTESIAN_POINT('Origin',(69.8343145750508,0.,0.));
#12131=CARTESIAN_POINT('',(70.1171572875254,-1.33276384934561E-15,10.8828427124746));
#12132=CARTESIAN_POINT('',(70.1171572875254,-10.8828427124746,-1.33276384934562E-15));
#12133=CARTESIAN_POINT('Origin',(70.1171572875254,0.,-1.66595481168202E-15));
#12134=CARTESIAN_POINT('Origin',(70.1171572875254,0.,-1.66595481168202E-15));
#12135=CARTESIAN_POINT('',(69.8343145750508,-1.34711147906209E-15,11.));
#12136=CARTESIAN_POINT('Origin',(69.8343145750508,-1.29812560709619E-15,
10.6));
#12137=CARTESIAN_POINT('',(69.8343145750508,-11.,-1.34711147906209E-15));
#12138=CARTESIAN_POINT('Origin',(69.8343145750508,0.,0.));
#12139=CARTESIAN_POINT('Origin',(69.8343145750508,0.,0.));
#12140=CARTESIAN_POINT('Origin',(68.9,0.,0.));
#12141=CARTESIAN_POINT('',(68.9,-11.,-1.34711147906209E-15));
#12142=CARTESIAN_POINT('Origin',(70.25,0.,0.));
#12143=CARTESIAN_POINT('',(70.3828427124746,-10.6171572875254,-1.3002267688212E-15));
#12144=CARTESIAN_POINT('',(70.3828427124746,-1.3002267688212E-15,10.6171572875254));
#12145=CARTESIAN_POINT('Origin',(70.3828427124746,0.,-1.62528346102649E-15));
#12146=CARTESIAN_POINT('',(70.25,-10.75,-1.3164953090834E-15));
#12147=CARTESIAN_POINT('Origin',(70.3828427124746,0.,-1.62528346102649E-15));
#12148=CARTESIAN_POINT('Origin',(66.6,0.,0.));
#12149=CARTESIAN_POINT('',(66.6,-1.34711147906209E-15,11.));
#12150=CARTESIAN_POINT('Origin',(66.6,-1.29812560709619E-15,10.6));
#12151=CARTESIAN_POINT('',(66.6,-11.,-1.34711147906209E-15));
#12152=CARTESIAN_POINT('Origin',(66.6,0.,0.));
#12153=CARTESIAN_POINT('Origin',(66.6,0.,0.));
#12154=CARTESIAN_POINT('Origin',(58.1,0.,0.));
#12155=CARTESIAN_POINT('',(49.3656854249492,-11.,-1.34711147906209E-15));
#12156=CARTESIAN_POINT('',(58.1,-11.,-1.34711147906209E-15));
#12157=CARTESIAN_POINT('',(49.3656854249492,10.7121426428143,-2.5));
#12158=CARTESIAN_POINT('Origin',(49.3656854249492,0.,0.));
#12159=CARTESIAN_POINT('',(58.1,10.7121426428143,-2.5));
#12160=CARTESIAN_POINT('Origin',(49.3656854249492,0.,0.));
#12161=CARTESIAN_POINT('Origin',(49.3656854249492,0.,0.));
#12162=CARTESIAN_POINT('',(49.290874720642,10.7048947780099,-2.50000000016032));
#12163=CARTESIAN_POINT('Ctrl Pts',(49.2908747204936,10.7048947787685,-2.5));
#12164=CARTESIAN_POINT('Ctrl Pts',(49.3162118393145,10.7098484152371,-2.5));
#12165=CARTESIAN_POINT('Ctrl Pts',(49.3420008434342,10.7121426428143,-2.5));
#12166=CARTESIAN_POINT('Ctrl Pts',(49.3656854249492,10.7121426428143,-2.5));
#12167=CARTESIAN_POINT('',(49.3323331704973,10.6616743509686,2.70149187398907));
#12168=CARTESIAN_POINT('Ctrl Pts',(49.2908747206827,10.7048947779969,2.4999999991104));
#12169=CARTESIAN_POINT('Ctrl Pts',(49.3045010041015,10.6906254142154,2.5724257382579));
#12170=CARTESIAN_POINT('Ctrl Pts',(49.3184413442248,10.6761441724483,2.63964675585704));
#12171=CARTESIAN_POINT('Ctrl Pts',(49.3323950806311,10.6616812501835,2.70147713019892));
#12172=CARTESIAN_POINT('',(49.0828426943265,10.4676389273726,2.97738149942411));
#12173=CARTESIAN_POINT('Ctrl Pts',(49.3324087881176,10.6616015016905,2.70162046046199));
#12174=CARTESIAN_POINT('Ctrl Pts',(49.3135649567906,10.6557614583055,2.71827621407867));
#12175=CARTESIAN_POINT('Ctrl Pts',(49.2952674330737,10.6484809566042,2.73524347292328));
#12176=CARTESIAN_POINT('Ctrl Pts',(49.2776083070661,10.6399566490912,2.75232179660182));
#12177=CARTESIAN_POINT('Ctrl Pts',(49.2689844692774,10.6357938017781,2.76066199945467));
#12178=CARTESIAN_POINT('Ctrl Pts',(49.2605129098377,10.6313342979202,2.76902953786562));
#12179=CARTESIAN_POINT('Ctrl Pts',(49.2522046371122,10.626600777531,2.77740545786278));
#12180=CARTESIAN_POINT('Ctrl Pts',(49.2346176799969,10.6165808584889,2.79513561076665));
#12181=CARTESIAN_POINT('Ctrl Pts',(49.217760859958,10.6053345841082,2.81290035916848));
#12182=CARTESIAN_POINT('Ctrl Pts',(49.2016912137775,10.5931223499357,2.83054337312961));
#12183=CARTESIAN_POINT('Ctrl Pts',(49.199028540575,10.5910988337793,2.83346674679688));
#12184=CARTESIAN_POINT('Ctrl Pts',(49.1963875221415,10.5890487558497,2.83638687761696));
#12185=CARTESIAN_POINT('Ctrl Pts',(49.1937684684831,10.5869732520537,2.83930316752249));
#12186=CARTESIAN_POINT('Ctrl Pts',(49.1749952468881,10.5720961636983,2.86020696094277));
#12187=CARTESIAN_POINT('Ctrl Pts',(49.1571526657491,10.5557556236773,2.88110859508633));
#12188=CARTESIAN_POINT('Ctrl Pts',(49.1403287769875,10.5381710427577,2.90181519954335));
#12189=CARTESIAN_POINT('Ctrl Pts',(49.12259672862,10.5196372397941,2.92363955400515));
#12190=CARTESIAN_POINT('Ctrl Pts',(49.1059960732651,10.4997217021854,2.94524832138529));
#12191=CARTESIAN_POINT('Ctrl Pts',(49.090663937318,10.4786485987581,2.96644693548253));
#12192=CARTESIAN_POINT('Ctrl Pts',(49.0884574234901,10.4756158775333,2.9694977194893));
#12193=CARTESIAN_POINT('Ctrl Pts',(49.0862772408328,10.4725591253496,2.97254004233701));
#12194=CARTESIAN_POINT('Ctrl Pts',(49.0841238569374,10.4694789537369,2.97557335278404));
#12195=CARTESIAN_POINT('Ctrl Pts',(49.083695781619,10.4688666405089,2.97617635039085));
#12196=CARTESIAN_POINT('Ctrl Pts',(49.0832687102321,10.4682533253048,2.97677906069511));
#12197=CARTESIAN_POINT('Ctrl Pts',(49.0828426468962,10.4676390119166,2.97738147896229));
#12198=CARTESIAN_POINT('',(49.0828426943265,10.4676389273726,-2.97738149942411));
#12199=CARTESIAN_POINT('Origin',(49.0828427124746,0.,-1.66595481168202E-15));
#12200=CARTESIAN_POINT('',(49.3323331704973,10.6616743509686,-2.70149187398906));
#12201=CARTESIAN_POINT('Ctrl Pts',(49.0828426468962,10.4676390119166,-2.97738147896229));
#12202=CARTESIAN_POINT('Ctrl Pts',(49.0832687102357,10.46825332531,-2.97677906068993));
#12203=CARTESIAN_POINT('Ctrl Pts',(49.0836957816155,10.4688666405034,-2.9761763503977));
#12204=CARTESIAN_POINT('Ctrl Pts',(49.0841238569375,10.4694789537365,-2.97557335278547));
#12205=CARTESIAN_POINT('Ctrl Pts',(49.0997803379974,10.4918737755011,-2.95351924171713));
#12206=CARTESIAN_POINT('Ctrl Pts',(49.1168500766551,10.5130338506644,-2.93098701763205));
#12207=CARTESIAN_POINT('Ctrl Pts',(49.1351711977364,10.5327069760909,-2.90819678821397));
#12208=CARTESIAN_POINT('Ctrl Pts',(49.1517839963378,10.5505457136398,-2.88753159585364));
#12209=CARTESIAN_POINT('Ctrl Pts',(49.169426161142,10.5671614160477,-2.86665343070936));
#12210=CARTESIAN_POINT('Ctrl Pts',(49.1880067011391,10.5823374979221,-2.8457516840311));
#12211=CARTESIAN_POINT('Ctrl Pts',(49.1899173698306,10.5838980803649,-2.84360232168846));
#12212=CARTESIAN_POINT('Ctrl Pts',(49.1918379861858,10.5854434157622,-2.84145274014321));
#12213=CARTESIAN_POINT('Ctrl Pts',(49.1937684684827,10.5869732520534,-2.83930316752288));
#12214=CARTESIAN_POINT('Ctrl Pts',(49.209574863942,10.5994992397022,-2.82170290516363));
#12215=CARTESIAN_POINT('Ctrl Pts',(49.2261797406536,10.6111006259049,-2.80395929532978));
#12216=CARTESIAN_POINT('Ctrl Pts',(49.243522871543,10.621520087492,-2.78622125562479));
#12217=CARTESIAN_POINT('Ctrl Pts',(49.2463965558388,10.6232465487248,-2.78328213658884));
#12218=CARTESIAN_POINT('Ctrl Pts',(49.2492905518298,10.6249405188279,-2.78034327008876));
#12219=CARTESIAN_POINT('Ctrl Pts',(49.2522046371122,10.626600777531,-2.77740545786278));
#12220=CARTESIAN_POINT('Ctrl Pts',(49.2692175771233,10.6362936584803,-2.76025399580113));
#12221=CARTESIAN_POINT('Ctrl Pts',(49.2869149560756,10.6448377817445,-2.74313460503217));
#12222=CARTESIAN_POINT('Ctrl Pts',(49.3052032408308,10.6520378277433,-2.7262223666424));
#12223=CARTESIAN_POINT('Ctrl Pts',(49.3141343284223,10.6555539716759,-2.7179632715742));
#12224=CARTESIAN_POINT('Ctrl Pts',(49.3232063992444,10.6587495153119,-2.70975430113892));
#12225=CARTESIAN_POINT('Ctrl Pts',(49.3324087881176,10.6616015016905,-2.70162046046199));
#12226=CARTESIAN_POINT('Ctrl Pts',(49.3323950806311,10.6616812501835,-2.70147713019892));
#12227=CARTESIAN_POINT('Ctrl Pts',(49.317580223994,10.677037679497,-2.63583083212022));
#12228=CARTESIAN_POINT('Ctrl Pts',(49.3037413307877,10.6914388937186,-2.56837430025778));
#12229=CARTESIAN_POINT('Ctrl Pts',(49.2908747206929,10.7048947779706,-2.49999999917371));
#12230=CARTESIAN_POINT('Origin',(48.95,0.,0.));
#12231=CARTESIAN_POINT('',(48.8171572875254,10.1905533656526,2.97937090169063));
#12232=CARTESIAN_POINT('Ctrl Pts',(48.8171572875336,10.1905533656612,2.97937090169057));
#12233=CARTESIAN_POINT('Ctrl Pts',(48.9056698328978,10.2829700356906,2.97869109651476));
#12234=CARTESIAN_POINT('Ctrl Pts',(48.9942328602291,10.3753305077211,2.97802834000757));
#12235=CARTESIAN_POINT('Ctrl Pts',(49.0828426330983,10.4676389975428,2.97738147906302));
#12236=CARTESIAN_POINT('',(48.8171572875336,10.1905533656612,-2.97937090169057));
#12237=CARTESIAN_POINT('Origin',(48.8171572875254,0.,-1.62528346102649E-15));
#12238=CARTESIAN_POINT('Ctrl Pts',(49.0828426330983,10.4676389975428,-2.97738147906302));
#12239=CARTESIAN_POINT('Ctrl Pts',(48.9942328602291,10.3753305077211,-2.97802834000757));
#12240=CARTESIAN_POINT('Ctrl Pts',(48.9056698328978,10.2829700356906,-2.97869109651476));
#12241=CARTESIAN_POINT('Ctrl Pts',(48.8171572875336,10.1905533656612,-2.97937090169057));
#12242=CARTESIAN_POINT('Ctrl Pts',(48.8171572875336,10.1905533656612,2.97937090169057));
#12243=CARTESIAN_POINT('Ctrl Pts',(48.9778062289061,10.3582882347049,2.97813706549952));
#12244=CARTESIAN_POINT('Ctrl Pts',(49.1386214664861,10.5258379779574,2.97695939052998));
#12245=CARTESIAN_POINT('Ctrl Pts',(49.2995806606493,10.6932278010799,2.97583098251121));
#12246=CARTESIAN_POINT('Ctrl Pts',(48.8075014991423,10.1998211785253,2.91326259488353));
#12247=CARTESIAN_POINT('Ctrl Pts',(48.9683243751193,10.3674015107644,2.91210397456444));
#12248=CARTESIAN_POINT('Ctrl Pts',(49.1293028626815,10.5348051777809,2.9109997011877));
#12249=CARTESIAN_POINT('Ctrl Pts',(49.2904188809618,10.7020541703147,2.90994206251764));
#12250=CARTESIAN_POINT('Ctrl Pts',(48.8129307052331,10.1946101212806,2.77448556461726));
#12251=CARTESIAN_POINT('Ctrl Pts',(48.9740100519798,10.3619373600493,2.773609368412));
#12252=CARTESIAN_POINT('Ctrl Pts',(49.1352307428308,10.5291011568935,2.77277138099925));
#12253=CARTESIAN_POINT('Ctrl Pts',(49.2965774530089,10.696121062043,2.77197377859995));
#12254=CARTESIAN_POINT('Ctrl Pts',(48.9060750398012,10.1052083834689,2.5673532928901));
#12255=CARTESIAN_POINT('Ctrl Pts',(49.0671873646562,10.2723851179806,2.56710210511172));
#12256=CARTESIAN_POINT('Ctrl Pts',(49.228440291876,10.4394075522319,2.56686429820521));
#12257=CARTESIAN_POINT('Ctrl Pts',(49.3898161252289,10.6062958341897,2.56663635849247));
#12258=CARTESIAN_POINT('Ctrl Pts',(49.0270075945874,9.98913497324999,2.5));
#12259=CARTESIAN_POINT('Ctrl Pts',(49.1878342329928,10.1564318375549,2.5000050401676));
#12260=CARTESIAN_POINT('Ctrl Pts',(49.3488133909105,10.3235745081665,2.4999954671014));
#12261=CARTESIAN_POINT('Ctrl Pts',(49.509932319593,10.490577063526,2.5));
#12262=CARTESIAN_POINT('Ctrl Pts',(49.1000000000083,9.91907544765526,2.5));
#12263=CARTESIAN_POINT('Ctrl Pts',(49.2606489413807,10.0864495849984,2.5));
#12264=CARTESIAN_POINT('Ctrl Pts',(49.4214641789608,10.2536640921303,2.5));
#12265=CARTESIAN_POINT('Ctrl Pts',(49.582423373124,10.4207398892537,2.5));
#12266=CARTESIAN_POINT('Ctrl Pts',(49.471102006026,10.3051417027149,2.5));
#12267=CARTESIAN_POINT('Ctrl Pts',(49.4519249796202,10.3173672432757,2.49999972617162));
#12268=CARTESIAN_POINT('Ctrl Pts',(49.4342238284002,10.3311503742156,2.50195700947107));
#12269=CARTESIAN_POINT('Ctrl Pts',(49.4181923288807,10.3463856016532,2.50579886168802));
#12270=CARTESIAN_POINT('Ctrl Pts',(49.4094187675144,10.354723387067,2.50790139277969));
#12271=CARTESIAN_POINT('Ctrl Pts',(49.4011454590667,10.363495905895,2.51056922958518));
#12272=CARTESIAN_POINT('Ctrl Pts',(49.3934065141206,10.3726836074799,2.51379620007939));
#12273=CARTESIAN_POINT('Ctrl Pts',(49.3810666011945,10.3873335937945,2.51894167342119));
#12274=CARTESIAN_POINT('Ctrl Pts',(49.3704042965574,10.4026552679914,2.5253725502872));
#12275=CARTESIAN_POINT('Ctrl Pts',(49.3613432382584,10.4184314703273,2.5328774372176));
#12276=CARTESIAN_POINT('Ctrl Pts',(49.3541440763532,10.4309659261399,2.53884019502236));
#12277=CARTESIAN_POINT('Ctrl Pts',(49.3479550864531,10.4437879009631,2.54548197767861));
#12278=CARTESIAN_POINT('Ctrl Pts',(49.342728971544,10.4567969890248,2.55271641212372));
#12279=CARTESIAN_POINT('Ctrl Pts',(49.3360883735995,10.4733270739819,2.56190889475026));
#12280=CARTESIAN_POINT('Ctrl Pts',(49.3310669542557,10.4899794155241,2.57196098389177));
#12281=CARTESIAN_POINT('Ctrl Pts',(49.3275006077779,10.5065537921764,2.58265564561844));
#12282=CARTESIAN_POINT('Ctrl Pts',(49.3247047093136,10.5195475589116,2.5910399090332));
#12283=CARTESIAN_POINT('Ctrl Pts',(49.3228024401235,10.5324940401409,2.59982007462608));
#12284=CARTESIAN_POINT('Ctrl Pts',(49.3217047589493,10.5453062357258,2.60890897643727));
#12285=CARTESIAN_POINT('Ctrl Pts',(49.3210833200784,10.5525597047164,2.61405454785858));
#12286=CARTESIAN_POINT('Ctrl Pts',(49.3207195791288,10.5597703070915,2.61929926750326));
#12287=CARTESIAN_POINT('Ctrl Pts',(49.320593282732,10.5669261888948,2.62462354576028));
#12288=CARTESIAN_POINT('Ctrl Pts',(49.3202452202704,10.5866472094313,2.63929681786496));
#12289=CARTESIAN_POINT('Ctrl Pts',(49.321698592633,10.6065613171611,2.65501534839773));
#12290=CARTESIAN_POINT('Ctrl Pts',(49.3249307613735,10.6265525087281,2.67163246997651));
#12291=CARTESIAN_POINT('Ctrl Pts',(49.3268169984925,10.6382190183124,2.68132993135651));
#12292=CARTESIAN_POINT('Ctrl Pts',(49.3293095351321,10.649911295547,2.69133415471351));
#12293=CARTESIAN_POINT('Ctrl Pts',(49.3324087878956,10.6616015010747,2.70162045999414));
#12294=CARTESIAN_POINT('Origin',(49.1000000000083,9.91907544765526,2.9));
#12295=CARTESIAN_POINT('Ctrl Pts',(49.462305708714,10.3051823273304,2.46082185490775));
#12296=CARTESIAN_POINT('Ctrl Pts',(49.4771037846566,10.3051138491653,2.52723063922477));
#12297=CARTESIAN_POINT('Ctrl Pts',(49.49243661118,10.3050433229319,2.59347917296297));
#12298=CARTESIAN_POINT('Ctrl Pts',(49.5082942562487,10.3049708790319,2.65958704920729));
#12299=CARTESIAN_POINT('Ctrl Pts',(49.4083727211377,10.341288010494,2.47275277189045));
#12300=CARTESIAN_POINT('Ctrl Pts',(49.4232536647421,10.3411829551313,2.53945009831164));
#12301=CARTESIAN_POINT('Ctrl Pts',(49.4386713993083,10.3410740762491,2.60598280249336));
#12302=CARTESIAN_POINT('Ctrl Pts',(49.4546159715293,10.3409629277268,2.67237043888862));
#12303=CARTESIAN_POINT('Ctrl Pts',(49.3031992070178,10.4580767906371,2.49601898654185));
#12304=CARTESIAN_POINT('Ctrl Pts',(49.3182156131681,10.4578563589617,2.56328424053666));
#12305=CARTESIAN_POINT('Ctrl Pts',(49.3337734061097,10.4576291666046,2.63037822823133));
#12306=CARTESIAN_POINT('Ctrl Pts',(49.3498601387948,10.4573959072113,2.69731785735098));
#12307=CARTESIAN_POINT('Ctrl Pts',(49.2766718995763,10.6180800401588,2.50188728935765));
#12308=CARTESIAN_POINT('Ctrl Pts',(49.2916193758389,10.617743529058,2.56932146539533));
#12309=CARTESIAN_POINT('Ctrl Pts',(49.3071014259566,10.6173974045177,2.63657775200008));
#12310=CARTESIAN_POINT('Ctrl Pts',(49.3231160197943,10.6170409930902,2.70368692254473));
#12311=CARTESIAN_POINT('Ctrl Pts',(49.2906111221464,10.7049013470625,2.49880369034412));
#12312=CARTESIAN_POINT('Ctrl Pts',(49.3054535577802,10.7045314987806,2.5661795783969));
#12313=CARTESIAN_POINT('Ctrl Pts',(49.3208320100222,10.7041502377578,2.63338623008397));
#12314=CARTESIAN_POINT('Ctrl Pts',(49.3367364522403,10.7037582059502,2.70044324036495));
#12315=CARTESIAN_POINT('Ctrl Pts',(49.5082942562487,10.3049708790319,-2.65958704920729));
#12316=CARTESIAN_POINT('Ctrl Pts',(49.4924395390992,10.3050433095561,-2.59349137896939));
#12317=CARTESIAN_POINT('Ctrl Pts',(49.4771094475134,10.305113823118,-2.52725510661945));
#12318=CARTESIAN_POINT('Ctrl Pts',(49.4623139056172,10.3051822893992,-2.46085863958849));
#12319=CARTESIAN_POINT('Ctrl Pts',(49.4546159715295,10.3409629277267,-2.67237043888858));
#12320=CARTESIAN_POINT('Ctrl Pts',(49.4386743432776,10.3410740557268,-2.60599506015401));
#12321=CARTESIAN_POINT('Ctrl Pts',(49.4232593589763,10.3411829150475,-2.53947467065603));
#12322=CARTESIAN_POINT('Ctrl Pts',(49.4083809639253,10.3412879521802,-2.47278971640008));
#12323=CARTESIAN_POINT('Ctrl Pts',(49.3498601387952,10.4573959072108,-2.69731785735089));
#12324=CARTESIAN_POINT('Ctrl Pts',(49.3337763763275,10.4576291235356,-2.6303905878106));
#12325=CARTESIAN_POINT('Ctrl Pts',(49.3182213589273,10.4578562750788,-2.56330901994368));
#12326=CARTESIAN_POINT('Ctrl Pts',(49.3032075250344,10.4580766685106,-2.49605624588246));
#12327=CARTESIAN_POINT('Ctrl Pts',(49.3231160197944,10.6170409930891,-2.7036869225447));
#12328=CARTESIAN_POINT('Ctrl Pts',(49.3071043828546,10.6173973387096,-2.63659014288315));
#12329=CARTESIAN_POINT('Ctrl Pts',(49.2916250945902,10.6177434011025,-2.56934630598959));
#12330=CARTESIAN_POINT('Ctrl Pts',(49.2766801784892,10.6180798538746,-2.50192464095437));
#12331=CARTESIAN_POINT('Ctrl Pts',(49.3367364522401,10.7037582059489,-2.700443240365));
#12332=CARTESIAN_POINT('Ctrl Pts',(49.3208349465817,10.7041501653727,-2.63339861133636));
#12333=CARTESIAN_POINT('Ctrl Pts',(49.3054592374878,10.7045313579687,-2.56620439965167));
#12334=CARTESIAN_POINT('Ctrl Pts',(49.2906193436209,10.7049011421962,-2.49884101071544));
#12335=CARTESIAN_POINT('',(49.4711020394073,10.3051416724427,-2.5));
#12336=CARTESIAN_POINT('Ctrl Pts',(49.3323950805385,10.6616812492885,-2.70147713001029));
#12337=CARTESIAN_POINT('Ctrl Pts',(49.3271569720922,10.6417619720421,-2.68393641922588));
#12338=CARTESIAN_POINT('Ctrl Pts',(49.3237005583529,10.6218293402928,-2.66722269704707));
#12339=CARTESIAN_POINT('Ctrl Pts',(49.3219885926706,10.6020145351385,-2.65145685176126));
#12340=CARTESIAN_POINT('Ctrl Pts',(49.3209757435438,10.5902915150407,-2.64212931511863));
#12341=CARTESIAN_POINT('Ctrl Pts',(49.3205744428189,10.5786096190675,-2.63313320519147));
#12342=CARTESIAN_POINT('Ctrl Pts',(49.3207850049258,10.5669968946579,-2.62449066979262));
#12343=CARTESIAN_POINT('Ctrl Pts',(49.3210756127816,10.550969561956,-2.6125626514104));
#12344=CARTESIAN_POINT('Ctrl Pts',(49.3225361848226,10.5346775925373,-2.60100536084123));
#12345=CARTESIAN_POINT('Ctrl Pts',(49.3253648341183,10.5182626775943,-2.59003870410598));
#12346=CARTESIAN_POINT('Ctrl Pts',(49.3280417284346,10.5027284109103,-2.57966040053581));
#12347=CARTESIAN_POINT('Ctrl Pts',(49.331943942577,10.4870838027976,-2.56981112723947));
#12348=CARTESIAN_POINT('Ctrl Pts',(49.3372505335242,10.4714944194039,-2.5606726536798));
#12349=CARTESIAN_POINT('Ctrl Pts',(49.338907744272,10.466625965444,-2.55781877314679));
#12350=CARTESIAN_POINT('Ctrl Pts',(49.3407019993306,10.4617632603077,-2.55503417504958));
#12351=CARTESIAN_POINT('Ctrl Pts',(49.3426389695942,10.4569123869465,-2.55232427803795));
#12352=CARTESIAN_POINT('Ctrl Pts',(49.3436752717814,10.4543171118569,-2.55087445082417));
#12353=CARTESIAN_POINT('Ctrl Pts',(49.3447507774767,10.451729479217,-2.54944858395426));
#12354=CARTESIAN_POINT('Ctrl Pts',(49.3458660878379,10.4491502726166,-2.54804741897205));
#12355=CARTESIAN_POINT('Ctrl Pts',(49.3528539912289,10.4329904240435,-2.53926851233641));
#12356=CARTESIAN_POINT('Ctrl Pts',(49.3614046849159,10.4171575527942,-2.5314598314099));
#12357=CARTESIAN_POINT('Ctrl Pts',(49.3715767266835,10.4018302197805,-2.52481994804416));
#12358=CARTESIAN_POINT('Ctrl Pts',(49.3781479620868,10.3919286173649,-2.52053052045005));
#12359=CARTESIAN_POINT('Ctrl Pts',(49.385395823602,10.3822388736403,-2.51672872957607));
#12360=CARTESIAN_POINT('Ctrl Pts',(49.3933348932719,10.3728207109584,-2.51346660440115));
#12361=CARTESIAN_POINT('Ctrl Pts',(49.4070771902143,10.3565181473573,-2.50781996132063));
#12362=CARTESIAN_POINT('Ctrl Pts',(49.4224925047283,10.3414985031374,-2.50395905075391));
#12363=CARTESIAN_POINT('Ctrl Pts',(49.4393853211129,10.327896747852,-2.50186576538707));
#12364=CARTESIAN_POINT('Ctrl Pts',(49.4494441471084,10.3197975838917,-2.50061931880381));
#12365=CARTESIAN_POINT('Ctrl Pts',(49.4600277835471,10.3122015103339,-2.49999924910275));
#12366=CARTESIAN_POINT('Ctrl Pts',(49.4711018430278,10.3051416733453,-2.49999916367266));
#12367=CARTESIAN_POINT('Ctrl Pts',(49.2908747205623,10.7048947773287,-2.499999999072));
#12368=CARTESIAN_POINT('Ctrl Pts',(49.2872058781153,10.6831077488647,-2.49999977996358));
#12369=CARTESIAN_POINT('Ctrl Pts',(49.2854473079225,10.6610039750184,-2.49998517158562));
#12370=CARTESIAN_POINT('Ctrl Pts',(49.2855726481819,10.6388034196963,-2.49997268059858));
#12371=CARTESIAN_POINT('Ctrl Pts',(49.2856981913103,10.6165669317439,-2.49996016939429));
#12372=CARTESIAN_POINT('Ctrl Pts',(49.2877121963881,10.5944414635718,-2.49994942515778));
#12373=CARTESIAN_POINT('Ctrl Pts',(49.2915330177167,10.5726477963842,-2.49994809325073));
#12374=CARTESIAN_POINT('Ctrl Pts',(49.2953838688655,10.5506828414414,-2.49994675087554));
#12375=CARTESIAN_POINT('Ctrl Pts',(49.3010702648263,10.5290535111454,-2.49995491240654));
#12376=CARTESIAN_POINT('Ctrl Pts',(49.3085583741435,10.5079899006643,-2.49996733309932));
#12377=CARTESIAN_POINT('Ctrl Pts',(49.3107658785906,10.5017803206703,-2.49997099473584));
#12378=CARTESIAN_POINT('Ctrl Pts',(49.3131302814176,10.4956200105166,-2.49997494360772));
#12379=CARTESIAN_POINT('Ctrl Pts',(49.3156514926051,10.4895152119484,-2.49997884080595));
#12380=CARTESIAN_POINT('Ctrl Pts',(49.3213480167851,10.4757217888387,-2.49998764628964));
#12381=CARTESIAN_POINT('Ctrl Pts',(49.3278098816835,10.4622952988396,-2.49999625392971));
#12382=CARTESIAN_POINT('Ctrl Pts',(49.3350146013469,10.4492980432451,-2.50000038352441));
#12383=CARTESIAN_POINT('Ctrl Pts',(49.3458363826384,10.4297756379321,-2.50000658634322));
#12384=CARTESIAN_POINT('Ctrl Pts',(49.3583318951607,10.4112200704296,-2.50000320120766));
#12385=CARTESIAN_POINT('Ctrl Pts',(49.3723085264239,10.393783414394,-2.50000070356517));
#12386=CARTESIAN_POINT('Ctrl Pts',(49.3817076056388,10.3820575193457,-2.49999902393729));
#12387=CARTESIAN_POINT('Ctrl Pts',(49.3917776159901,10.3708379724724,-2.49999747922745));
#12388=CARTESIAN_POINT('Ctrl Pts',(49.4024704737568,10.3601786152418,-2.49999676540344));
#12389=CARTESIAN_POINT('Ctrl Pts',(49.4184910300295,10.3442082510913,-2.49999569591783));
#12390=CARTESIAN_POINT('Ctrl Pts',(49.4357738390234,10.3296276305099,-2.49999714156594));
#12391=CARTESIAN_POINT('Ctrl Pts',(49.4541233624076,10.3165800826316,-2.499998440249));
#12392=CARTESIAN_POINT('Ctrl Pts',(49.4596860976899,10.3126246635502,-2.49999883395024));
#12393=CARTESIAN_POINT('Ctrl Pts',(49.4653471679471,10.308810334878,-2.49999915006047));
#12394=CARTESIAN_POINT('Ctrl Pts',(49.4711018430278,10.3051416733453,-2.49999916367266));
#12395=CARTESIAN_POINT('Ctrl Pts',(49.2995806606493,10.6932278010799,-2.97583098251121));
#12396=CARTESIAN_POINT('Ctrl Pts',(49.1386214664862,10.5258379779574,-2.97695939052998));
#12397=CARTESIAN_POINT('Ctrl Pts',(48.9778062289061,10.3582882347048,-2.97813706549952));
#12398=CARTESIAN_POINT('Ctrl Pts',(48.8171572875336,10.1905533656612,-2.97937090169057));
#12399=CARTESIAN_POINT('Ctrl Pts',(49.2904188809618,10.7020541703147,-2.90994206251764));
#12400=CARTESIAN_POINT('Ctrl Pts',(49.1293028626815,10.534805177781,-2.9109997011877));
#12401=CARTESIAN_POINT('Ctrl Pts',(48.9683243751193,10.3674015107643,-2.91210397456444));
#12402=CARTESIAN_POINT('Ctrl Pts',(48.8075014991423,10.1998211785253,-2.91326259488353));
#12403=CARTESIAN_POINT('Ctrl Pts',(49.2965774530089,10.696121062043,-2.77197377859995));
#12404=CARTESIAN_POINT('Ctrl Pts',(49.1352307428308,10.5291011568935,-2.77277138099925));
#12405=CARTESIAN_POINT('Ctrl Pts',(48.9740100519798,10.3619373600493,-2.773609368412));
#12406=CARTESIAN_POINT('Ctrl Pts',(48.8129307052331,10.1946101212806,-2.77448556461726));
#12407=CARTESIAN_POINT('Ctrl Pts',(49.3898161252289,10.6062958341897,-2.56663635849247));
#12408=CARTESIAN_POINT('Ctrl Pts',(49.228440291876,10.439407552232,-2.5668642982052));
#12409=CARTESIAN_POINT('Ctrl Pts',(49.0671873646562,10.2723851179806,-2.56710210511172));
#12410=CARTESIAN_POINT('Ctrl Pts',(48.9060750398012,10.1052083834689,-2.5673532928901));
#12411=CARTESIAN_POINT('Ctrl Pts',(49.509932319593,10.490577063526,-2.5));
#12412=CARTESIAN_POINT('Ctrl Pts',(49.3488133909105,10.3235745081665,-2.4999954671014));
#12413=CARTESIAN_POINT('Ctrl Pts',(49.1878342329928,10.1564318375549,-2.50000504016761));
#12414=CARTESIAN_POINT('Ctrl Pts',(49.0270075945874,9.98913497324999,-2.5));
#12415=CARTESIAN_POINT('Ctrl Pts',(49.582423373124,10.4207398892537,-2.5));
#12416=CARTESIAN_POINT('Ctrl Pts',(49.4214641789608,10.2536640921303,-2.5));
#12417=CARTESIAN_POINT('Ctrl Pts',(49.2606489413807,10.0864495849984,-2.5));
#12418=CARTESIAN_POINT('Ctrl Pts',(49.1000000000083,9.91907544765526,-2.5));
#12419=CARTESIAN_POINT('',(49.1000000000041,9.91907544765526,-2.5));
#12420=CARTESIAN_POINT('Origin',(49.1000000000083,9.91907544765526,-2.9));
#12421=CARTESIAN_POINT('Ctrl Pts',(49.1000000000083,9.91907544765526,-2.5));
#12422=CARTESIAN_POINT('Ctrl Pts',(49.2236056134068,10.0478555238674,-2.5));
#12423=CARTESIAN_POINT('Ctrl Pts',(49.3473096739212,10.176541099224,-2.5));
#12424=CARTESIAN_POINT('Ctrl Pts',(49.471102006026,10.3051417027149,-2.5));
#12425=CARTESIAN_POINT('Origin',(49.1,0.,0.));
#12426=CARTESIAN_POINT('',(48.7,9.91907544764665,2.9));
#12427=CARTESIAN_POINT('Origin',(49.1,9.91907544764666,2.9));
#12428=CARTESIAN_POINT('',(48.7,9.91907544764665,-2.9));
#12429=CARTESIAN_POINT('Origin',(48.7,0.,0.));
#12430=CARTESIAN_POINT('Origin',(49.1,9.91907544764666,-2.9));
#12431=CARTESIAN_POINT('Origin',(49.1,9.91907544764666,-2.9));
#12432=CARTESIAN_POINT('Origin',(49.1,9.91907544764666,-2.9));
#12433=CARTESIAN_POINT('Origin',(49.1,9.91907544764666,2.9));
#12434=CARTESIAN_POINT('Origin',(49.1,9.91907544764666,2.9));
#12435=CARTESIAN_POINT('Origin',(58.5,8.62,-2.5));
#12436=CARTESIAN_POINT('',(69.,10.24,-2.5));
#12437=CARTESIAN_POINT('',(49.1,7.83022988168291,-2.5));
#12438=CARTESIAN_POINT('',(49.1,9.56,-2.5));
#12439=CARTESIAN_POINT('',(69.0218379181362,7.83022988168291,-2.5));
#12440=CARTESIAN_POINT('',(59.6,7.83022988168291,-2.5));
#12441=CARTESIAN_POINT('',(69.,7.9669630349337,-2.5));
#12442=CARTESIAN_POINT('Ctrl Pts',(69.,7.96696303493369,-2.5));
#12443=CARTESIAN_POINT('Ctrl Pts',(69.,7.92356314245502,-2.5));
#12444=CARTESIAN_POINT('Ctrl Pts',(69.0075947074924,7.87360329207051,-2.5));
#12445=CARTESIAN_POINT('Ctrl Pts',(69.0218379181362,7.83022988168291,-2.5));
#12446=CARTESIAN_POINT('',(69.,10.24,-2.5));
#12447=CARTESIAN_POINT('',(69.,7.,-2.5));
#12448=CARTESIAN_POINT('',(69.,10.24,-2.5));
#12449=CARTESIAN_POINT('Origin',(49.1,9.56,-2.9));
#12450=CARTESIAN_POINT('',(48.7,7.83022988168291,-2.9));
#12451=CARTESIAN_POINT('',(48.7,9.56,-2.9));
#12452=CARTESIAN_POINT('Origin',(49.1,7.83022988168291,-2.9));
#12453=CARTESIAN_POINT('Origin',(48.7,10.5,0.));
#12454=CARTESIAN_POINT('',(48.7,7.83022988168291,2.9));
#12455=CARTESIAN_POINT('',(48.7,9.56,2.9));
#12456=CARTESIAN_POINT('Origin',(48.7,0.,0.));
#12457=CARTESIAN_POINT('Origin',(49.1,9.56,2.9));
#12458=CARTESIAN_POINT('Origin',(49.1,7.83022988168291,2.9));
#12459=CARTESIAN_POINT('Origin',(70.1,0.,0.));
#12460=CARTESIAN_POINT('',(70.5,-1.26558852657178E-15,10.3343145750508));
#12461=CARTESIAN_POINT('Origin',(70.5,0.,0.));
#12462=CARTESIAN_POINT('Origin',(70.1,-1.26558852657178E-15,10.3343145750508));
#12463=CARTESIAN_POINT('Origin',(70.5,7.95,0.));
#12464=CARTESIAN_POINT('',(70.5,-1.02258007728804E-15,8.35));
#12465=CARTESIAN_POINT('Origin',(70.5,0.,0.));
#12466=CARTESIAN_POINT('Origin',(70.1,0.,0.));
#12467=CARTESIAN_POINT('',(70.1,-9.73594205322146E-16,7.95));
#12468=CARTESIAN_POINT('',(70.1,-7.95,-9.73594205322146E-16));
#12469=CARTESIAN_POINT('Origin',(70.1,0.,0.));
#12470=CARTESIAN_POINT('Origin',(70.1,0.,0.));
#12471=CARTESIAN_POINT('Origin',(70.1,-1.02258007728804E-15,8.35));
#12472=CARTESIAN_POINT('Origin',(59.6,0.,0.));
#12473=CARTESIAN_POINT('',(49.1,-7.95,-9.73594205322146E-16));
#12474=CARTESIAN_POINT('',(59.6,-7.95,-9.73594205322146E-16));
#12475=CARTESIAN_POINT('',(49.1,7.45512904902744,2.76107784431138));
#12476=CARTESIAN_POINT('Origin',(49.1,0.,0.));
#12477=CARTESIAN_POINT('',(69.4,7.45512904902744,2.76107784431138));
#12478=CARTESIAN_POINT('',(59.6,7.45512904902744,2.76107784431138));
#12479=CARTESIAN_POINT('',(69.4,7.45512904902744,-2.76107784431138));
#12480=CARTESIAN_POINT('Origin',(69.4,0.,0.));
#12481=CARTESIAN_POINT('',(49.1,7.45512904902744,-2.76107784431138));
#12482=CARTESIAN_POINT('',(59.6,7.45512904902744,-2.76107784431138));
#12483=CARTESIAN_POINT('Origin',(49.1,0.,0.));
#12484=CARTESIAN_POINT('Origin',(69.,10.24,0.));
#12485=CARTESIAN_POINT('',(69.,10.24,0.));
#12486=CARTESIAN_POINT('Origin',(49.1,7.83022988168291,-2.9));
#12487=CARTESIAN_POINT('Origin',(49.1,7.83022988168291,-2.9));
#12488=CARTESIAN_POINT('Origin',(49.1,7.83022988168291,-2.9));
#12489=CARTESIAN_POINT('Origin',(49.1,7.83022988168291,2.9));
#12490=CARTESIAN_POINT('Origin',(49.1,7.83022988168291,2.9));
#12491=CARTESIAN_POINT('Origin',(49.1,7.83022988168291,2.9));
#12492=CARTESIAN_POINT('Origin',(49.1,0.,0.));
#12493=CARTESIAN_POINT('Origin',(59.6,7.83022988168291,-2.9));
#12494=CARTESIAN_POINT('Ctrl Pts',(69.4,7.45512904902744,-2.76107784431138));
#12495=CARTESIAN_POINT('Ctrl Pts',(69.3990583301394,7.45544816645284,-2.76021620196651));
#12496=CARTESIAN_POINT('Ctrl Pts',(69.3981166569032,7.45577025393396,-2.75935565609771));
#12497=CARTESIAN_POINT('Ctrl Pts',(69.3240866264373,7.48132475515606,-2.69178981004436));
#12498=CARTESIAN_POINT('Ctrl Pts',(69.2523194411631,7.52398051258273,-2.6328664623909));
#12499=CARTESIAN_POINT('Ctrl Pts',(69.142314610906,7.62274186069682,-2.55365184512958));
#12500=CARTESIAN_POINT('Ctrl Pts',(69.1013968001416,7.67221396448289,-2.52842397830978));
#12501=CARTESIAN_POINT('Ctrl Pts',(69.0504474618219,7.75813083757979,-2.50509269239044));
#12502=CARTESIAN_POINT('Ctrl Pts',(69.0339490479658,7.79334908159564,-2.5));
#12503=CARTESIAN_POINT('Ctrl Pts',(69.0218379181362,7.83022988168291,-2.5));
#12504=CARTESIAN_POINT('Origin',(69.4,0.,0.));
#12505=CARTESIAN_POINT('Ctrl Pts',(69.4,7.45512904902744,2.76107784431138));
#12506=CARTESIAN_POINT('Ctrl Pts',(69.3990583301394,7.45544816645284,2.76021620196653));
#12507=CARTESIAN_POINT('Ctrl Pts',(69.3981166569034,7.45577025393397,2.75935565609769));
#12508=CARTESIAN_POINT('Ctrl Pts',(69.3240866264303,7.481324755157,2.69178981004185));
#12509=CARTESIAN_POINT('Ctrl Pts',(69.2523194411595,7.52398051258612,2.6328664623884));
#12510=CARTESIAN_POINT('Ctrl Pts',(69.1423146109063,7.62274186069636,2.55365184512979));
#12511=CARTESIAN_POINT('Ctrl Pts',(69.1013968001419,7.67221396448251,2.52842397830999));
#12512=CARTESIAN_POINT('Ctrl Pts',(69.0504474618222,7.75813083757931,2.50509269239052));
#12513=CARTESIAN_POINT('Ctrl Pts',(69.0339490479659,7.79334908159538,2.5));
#12514=CARTESIAN_POINT('Ctrl Pts',(69.0218379181362,7.83022988168291,2.5));
#12515=CARTESIAN_POINT('Origin',(69.,0.,0.));
#12516=CARTESIAN_POINT('Origin',(59.6,7.83022988168291,2.9));
#12517=CARTESIAN_POINT('Origin',(69.,7.,0.));
#12518=CARTESIAN_POINT('',(0.,0.,0.));
#12519=CARTESIAN_POINT('Origin',(42.,0.,0.));
#12520=CARTESIAN_POINT('',(42.5,-1.87283927301222E-15,15.2928932188134));
#12521=CARTESIAN_POINT('Origin',(42.5,0.,0.));
#12522=CARTESIAN_POINT('',(42.3535533905933,-1.91613707582399E-15,15.6464466094067));
#12523=CARTESIAN_POINT('Origin',(42.,-1.87283927301222E-15,15.2928932188134));
#12524=CARTESIAN_POINT('',(42.3535533905933,-15.6464466094067,-1.91613707582399E-15));
#12525=CARTESIAN_POINT('Origin',(42.3535533905933,0.,-2.39517134477999E-15));
#12526=CARTESIAN_POINT('Origin',(42.3535533905933,0.,-2.39517134477999E-15));
#12527=CARTESIAN_POINT('Origin',(42.25,0.,0.));
#12528=CARTESIAN_POINT('',(42.1464466094067,-15.8535533905933,-1.94150034149017E-15));
#12529=CARTESIAN_POINT('',(42.25,-15.75,-1.92881870865708E-15));
#12530=CARTESIAN_POINT('',(42.1464466094067,-1.94150034149017E-15,15.8535533905933));
#12531=CARTESIAN_POINT('Origin',(42.1464466094067,0.,-2.42687542686271E-15));
#12532=CARTESIAN_POINT('Origin',(42.1464466094067,0.,-2.42687542686271E-15));
#12533=CARTESIAN_POINT('Origin',(42.5,10.5,0.));
#12534=CARTESIAN_POINT('',(42.5,-1.34711147906209E-15,11.));
#12535=CARTESIAN_POINT('Origin',(42.5,0.,0.));
#12536=CARTESIAN_POINT('Origin',(41.7928932188135,0.,0.));
#12537=CARTESIAN_POINT('',(41.7928932188135,-1.95943487863577E-15,16.));
#12538=CARTESIAN_POINT('Origin',(41.7928932188135,-1.8982025386784E-15,
15.5));
#12539=CARTESIAN_POINT('',(41.7928932188135,-16.,-1.95943487863577E-15));
#12540=CARTESIAN_POINT('Origin',(41.7928932188135,0.,0.));
#12541=CARTESIAN_POINT('Origin',(41.7928932188135,0.,0.));
#12542=CARTESIAN_POINT('Origin',(38.,0.,0.));
#12543=CARTESIAN_POINT('',(34.5,-16.,-1.95943487863577E-15));
#12544=CARTESIAN_POINT('',(38.,-16.,-1.95943487863577E-15));
#12545=CARTESIAN_POINT('',(34.5,-1.95943487863577E-15,16.));
#12546=CARTESIAN_POINT('Origin',(34.5,0.,0.));
#12547=CARTESIAN_POINT('Origin',(34.5,0.,0.));
#12548=CARTESIAN_POINT('Origin',(34.5,0.,0.));
#12549=CARTESIAN_POINT('',(34.,-1.8982025386784E-15,15.5));
#12550=CARTESIAN_POINT('Origin',(34.5,-1.8982025386784E-15,15.5));
#12551=CARTESIAN_POINT('Origin',(34.,0.,0.));
#12552=CARTESIAN_POINT('Origin',(34.,16.,0.));
#12553=CARTESIAN_POINT('',(34.,-1.34711147906209E-15,11.));
#12554=CARTESIAN_POINT('Origin',(34.,0.,0.));
#12555=CARTESIAN_POINT('Origin',(34.5,0.,0.));
#12556=CARTESIAN_POINT('',(34.5,-1.28587913910472E-15,10.5));
#12557=CARTESIAN_POINT('Origin',(34.5,-1.34711147906209E-15,11.));
#12558=CARTESIAN_POINT('',(34.5,-10.5,-1.28587913910472E-15));
#12559=CARTESIAN_POINT('Origin',(34.5,0.,0.));
#12560=CARTESIAN_POINT('Origin',(34.5,0.,0.));
#12561=CARTESIAN_POINT('Origin',(38.25,0.,0.));
#12562=CARTESIAN_POINT('',(42.,-1.28587913910472E-15,10.5));
#12563=CARTESIAN_POINT('',(42.,-10.5,-1.28587913910472E-15));
#12564=CARTESIAN_POINT('Origin',(42.,0.,0.));
#12565=CARTESIAN_POINT('Origin',(42.,0.,0.));
#12566=CARTESIAN_POINT('',(38.25,-10.5,-1.28587913910472E-15));
#12567=CARTESIAN_POINT('Origin',(42.,0.,0.));
#12568=CARTESIAN_POINT('Origin',(42.,-1.34711147906209E-15,11.));
#12569=CARTESIAN_POINT('',(0.,0.,0.));
#12570=CARTESIAN_POINT('Origin',(28.75,0.,0.));
#12571=CARTESIAN_POINT('',(42.,-10.5,-1.28587913910472E-15));
#12572=CARTESIAN_POINT('Origin',(42.,0.,0.));
#12573=CARTESIAN_POINT('',(15.5,-10.5,-1.28587913910472E-15));
#12574=CARTESIAN_POINT('',(28.75,-10.5,-1.28587913910472E-15));
#12575=CARTESIAN_POINT('Origin',(15.5,0.,0.));
#12576=CARTESIAN_POINT('Origin',(42.,8.265,0.));
#12577=CARTESIAN_POINT('',(42.,-8.265,-1.01217057949529E-15));
#12578=CARTESIAN_POINT('Origin',(42.,0.,0.));
#12579=CARTESIAN_POINT('Origin',(41.85,0.,0.));
#12580=CARTESIAN_POINT('',(41.7,-7.965,-9.75431175520866E-16));
#12581=CARTESIAN_POINT('',(41.85,-8.115,-9.93800877508077E-16));
#12582=CARTESIAN_POINT('Origin',(41.7,0.,0.));
#12583=CARTESIAN_POINT('Origin',(28.75,0.,0.));
#12584=CARTESIAN_POINT('',(15.8,-7.965,-9.75431175520867E-16));
#12585=CARTESIAN_POINT('',(28.75,-7.965,-9.75431175520867E-16));
#12586=CARTESIAN_POINT('Origin',(15.8,0.,0.));
#12587=CARTESIAN_POINT('Origin',(15.65,0.,0.));
#12588=CARTESIAN_POINT('',(15.5,-8.265,-1.01217057949529E-15));
#12589=CARTESIAN_POINT('',(15.65,-8.115,-9.93800877508077E-16));
#12590=CARTESIAN_POINT('Origin',(15.5,0.,0.));
#12591=CARTESIAN_POINT('Origin',(15.5,10.5,0.));
#12592=CARTESIAN_POINT('',(0.,0.,0.));
#12593=CARTESIAN_POINT('Origin',(0.1,0.,0.));
#12594=CARTESIAN_POINT('',(0.2,-11.,-1.34711147906209E-15));
#12595=CARTESIAN_POINT('Origin',(0.2,0.,0.));
#12596=CARTESIAN_POINT('',(-2.08166817117217E-16,-10.8,-1.32261854307914E-15));
#12597=CARTESIAN_POINT('',(0.1,-10.9,-1.33486501107062E-15));
#12598=CARTESIAN_POINT('Origin',(0.,0.,0.));
#12599=CARTESIAN_POINT('Origin',(1.,0.,0.));
#12600=CARTESIAN_POINT('',(1.8,-11.,-1.34711147906209E-15));
#12601=CARTESIAN_POINT('Origin',(1.8,0.,0.));
#12602=CARTESIAN_POINT('',(1.,-11.,-1.34711147906209E-15));
#12603=CARTESIAN_POINT('Origin',(1.9,0.,0.));
#12604=CARTESIAN_POINT('',(2.,-10.8,-1.32261854307914E-15));
#12605=CARTESIAN_POINT('Origin',(2.,0.,0.));
#12606=CARTESIAN_POINT('',(1.9,-10.9,-1.33486501107062E-15));
#12607=CARTESIAN_POINT('Origin',(2.,8.,0.));
#12608=CARTESIAN_POINT('',(2.,-8.,-9.79717439317883E-16));
#12609=CARTESIAN_POINT('Origin',(2.,0.,0.));
#12610=CARTESIAN_POINT('Origin',(1.,0.,0.));
#12611=CARTESIAN_POINT('',(0.,-8.,-9.79717439317883E-16));
#12612=CARTESIAN_POINT('',(1.,-8.,-9.79717439317883E-16));
#12613=CARTESIAN_POINT('Origin',(0.,0.,0.));
#12614=CARTESIAN_POINT('Origin',(0.,10.8,0.));
#12615=CARTESIAN_POINT('',(0.,0.,0.));
#12616=CARTESIAN_POINT('Origin',(0.,9.7,3.1));
#12617=CARTESIAN_POINT('',(0.,9.7,3.95));
#12618=CARTESIAN_POINT('Origin',(0.,9.7,3.1));
#12619=CARTESIAN_POINT('',(1.,9.7,3.95));
#12620=CARTESIAN_POINT('',(0.,9.7,3.95));
#12621=CARTESIAN_POINT('Origin',(1.,9.7,3.1));
#12622=CARTESIAN_POINT('Origin',(0.,9.7,-3.1));
#12623=CARTESIAN_POINT('',(0.,9.7,-2.25));
#12624=CARTESIAN_POINT('Origin',(0.,9.7,-3.1));
#12625=CARTESIAN_POINT('',(1.,9.7,-2.25));
#12626=CARTESIAN_POINT('',(0.,9.7,-2.25));
#12627=CARTESIAN_POINT('Origin',(1.,9.7,-3.1));
#12628=CARTESIAN_POINT('Origin',(1.,7.6,0.));
#12629=CARTESIAN_POINT('',(1.,7.42967024840268,1.6));
#12630=CARTESIAN_POINT('',(1.,10.9,1.6));
#12631=CARTESIAN_POINT('',(1.,8.3,1.6));
#12632=CARTESIAN_POINT('',(1.,10.9,4.4));
#12633=CARTESIAN_POINT('',(1.,10.9,1.6));
#12634=CARTESIAN_POINT('',(1.,8.8684835231284,4.4));
#12635=CARTESIAN_POINT('',(1.,10.9,4.4));
#12636=CARTESIAN_POINT('',(1.,8.8684835231284,-4.4));
#12637=CARTESIAN_POINT('Origin',(1.,0.,0.));
#12638=CARTESIAN_POINT('',(1.,10.9,-4.4));
#12639=CARTESIAN_POINT('',(1.,10.9,-4.4));
#12640=CARTESIAN_POINT('',(1.,10.9,-1.6));
#12641=CARTESIAN_POINT('',(1.,10.9,-1.6));
#12642=CARTESIAN_POINT('',(1.,7.42967024840268,-1.6));
#12643=CARTESIAN_POINT('',(1.,7.3,-1.6));
#12644=CARTESIAN_POINT('Origin',(1.,0.,0.));
#12645=CARTESIAN_POINT('Origin',(0.,10.9,-1.6));
#12646=CARTESIAN_POINT('',(0.,10.9,-1.6));
#12647=CARTESIAN_POINT('',(0.,10.9,-1.6));
#12648=CARTESIAN_POINT('',(0.,7.42967024840268,-1.6));
#12649=CARTESIAN_POINT('',(0.,8.45,-1.6));
#12650=CARTESIAN_POINT('',(0.5,7.42967024840268,-1.6));
#12651=CARTESIAN_POINT('Origin',(0.,10.9,-4.4));
#12652=CARTESIAN_POINT('',(0.,10.9,-4.4));
#12653=CARTESIAN_POINT('',(0.,10.9,-1.6));
#12654=CARTESIAN_POINT('',(0.,10.9,-4.4));
#12655=CARTESIAN_POINT('Origin',(0.,8.3,-4.4));
#12656=CARTESIAN_POINT('',(0.,8.8684835231284,-4.4));
#12657=CARTESIAN_POINT('',(0.5,8.8684835231284,-4.4));
#12658=CARTESIAN_POINT('',(0.,10.9,-4.4));
#12659=CARTESIAN_POINT('Origin',(0.,9.9,0.));
#12660=CARTESIAN_POINT('',(0.,10.9,1.6));
#12661=CARTESIAN_POINT('',(0.,7.42967024840268,1.6));
#12662=CARTESIAN_POINT('',(0.,10.7,1.6));
#12663=CARTESIAN_POINT('Origin',(0.,0.,0.));
#12664=CARTESIAN_POINT('',(0.,8.8684835231284,4.4));
#12665=CARTESIAN_POINT('Origin',(0.,0.,0.));
#12666=CARTESIAN_POINT('',(0.,10.9,4.4));
#12667=CARTESIAN_POINT('',(0.,10.9,4.4));
#12668=CARTESIAN_POINT('',(0.,10.9,1.6));
#12669=CARTESIAN_POINT('Origin',(0.5,0.,0.));
#12670=CARTESIAN_POINT('',(0.5,8.8684835231284,4.4));
#12671=CARTESIAN_POINT('Origin',(0.,10.9,4.4));
#12672=CARTESIAN_POINT('',(0.,10.9,4.4));
#12673=CARTESIAN_POINT('Origin',(0.,8.3,1.6));
#12674=CARTESIAN_POINT('',(0.,10.9,1.6));
#12675=CARTESIAN_POINT('',(0.5,7.42967024840268,1.6));
#12676=CARTESIAN_POINT('Origin',(0.,10.9,1.6));
#12677=CARTESIAN_POINT('Origin',(0.5,0.,0.));
#12678=CARTESIAN_POINT('',(0.,0.,0.));
#12679=CARTESIAN_POINT('Origin',(7.75,9.94,2.25));
#12680=CARTESIAN_POINT('',(8.,9.69,2.25));
#12681=CARTESIAN_POINT('',(7.75,9.69,2.5));
#12682=CARTESIAN_POINT('',(8.,9.69,2.25));
#12683=CARTESIAN_POINT('',(7.75,9.94,2.25));
#12684=CARTESIAN_POINT('',(7.75,9.94,2.25));
#12685=CARTESIAN_POINT('',(7.75,9.69,2.5));
#12686=CARTESIAN_POINT('Origin',(8.,5.19,2.25));
#12687=CARTESIAN_POINT('',(7.75,4.94,2.25));
#12688=CARTESIAN_POINT('',(7.75,5.19,2.5));
#12689=CARTESIAN_POINT('',(7.75,4.94,2.25));
#12690=CARTESIAN_POINT('',(8.,5.19,2.25));
#12691=CARTESIAN_POINT('',(8.,5.19,2.25));
#12692=CARTESIAN_POINT('',(7.75,5.19,2.5));
#12693=CARTESIAN_POINT('Origin',(0.,9.69,2.25));
#12694=CARTESIAN_POINT('',(0.25,9.94,2.25));
#12695=CARTESIAN_POINT('',(0.25,9.69,2.5));
#12696=CARTESIAN_POINT('',(0.25,9.94,2.25));
#12697=CARTESIAN_POINT('',(0.,9.69,2.25));
#12698=CARTESIAN_POINT('',(0.,9.69,2.25));
#12699=CARTESIAN_POINT('',(0.25,9.69,2.5));
#12700=CARTESIAN_POINT('Origin',(8.,9.69,-2.25));
#12701=CARTESIAN_POINT('',(7.75,9.94,-2.25));
#12702=CARTESIAN_POINT('',(7.75,9.69,-2.5));
#12703=CARTESIAN_POINT('',(7.75,9.94,-2.25));
#12704=CARTESIAN_POINT('',(8.,9.69,-2.25));
#12705=CARTESIAN_POINT('',(8.,9.69,-2.25));
#12706=CARTESIAN_POINT('',(7.75,9.69,-2.5));
#12707=CARTESIAN_POINT('Origin',(7.875,9.815,0.));
#12708=CARTESIAN_POINT('',(8.,9.69,0.));
#12709=CARTESIAN_POINT('',(7.75,9.94,0.));
#12710=CARTESIAN_POINT('Origin',(0.25,4.94,2.25));
#12711=CARTESIAN_POINT('',(0.,5.19,2.25));
#12712=CARTESIAN_POINT('',(0.25,5.19,2.5));
#12713=CARTESIAN_POINT('',(0.,5.19,2.25));
#12714=CARTESIAN_POINT('',(0.25,4.94,2.25));
#12715=CARTESIAN_POINT('',(0.25,4.94,2.25));
#12716=CARTESIAN_POINT('',(0.25,5.19,2.5));
#12717=CARTESIAN_POINT('Origin',(7.75,4.94,-2.25));
#12718=CARTESIAN_POINT('',(8.,5.19,-2.25));
#12719=CARTESIAN_POINT('',(7.75,5.19,-2.5));
#12720=CARTESIAN_POINT('',(8.,5.19,-2.25));
#12721=CARTESIAN_POINT('',(7.75,4.94,-2.25));
#12722=CARTESIAN_POINT('',(7.75,4.94,-2.25));
#12723=CARTESIAN_POINT('',(7.75,5.19,-2.5));
#12724=CARTESIAN_POINT('Origin',(7.875,5.065,0.));
#12725=CARTESIAN_POINT('',(7.75,4.94,0.));
#12726=CARTESIAN_POINT('',(8.,5.19,0.));
#12727=CARTESIAN_POINT('Origin',(0.25,9.94,-2.25));
#12728=CARTESIAN_POINT('',(0.,9.69,-2.25));
#12729=CARTESIAN_POINT('',(0.25,9.69,-2.5));
#12730=CARTESIAN_POINT('',(0.,9.69,-2.25));
#12731=CARTESIAN_POINT('',(0.25,9.94,-2.25));
#12732=CARTESIAN_POINT('',(0.25,9.94,-2.25));
#12733=CARTESIAN_POINT('',(0.25,9.69,-2.5));
#12734=CARTESIAN_POINT('Origin',(0.125,9.815,0.));
#12735=CARTESIAN_POINT('',(0.,9.69,0.));
#12736=CARTESIAN_POINT('',(0.25,9.94,0.));
#12737=CARTESIAN_POINT('Origin',(6.,9.815,-2.375));
#12738=CARTESIAN_POINT('',(6.,9.69,-2.5));
#12739=CARTESIAN_POINT('',(6.,9.94,-2.25));
#12740=CARTESIAN_POINT('Origin',(0.,5.19,-2.25));
#12741=CARTESIAN_POINT('',(0.25,4.94,-2.25));
#12742=CARTESIAN_POINT('',(0.25,5.19,-2.5));
#12743=CARTESIAN_POINT('',(0.25,4.94,-2.25));
#12744=CARTESIAN_POINT('',(0.,5.19,-2.25));
#12745=CARTESIAN_POINT('',(0.,5.19,-2.25));
#12746=CARTESIAN_POINT('',(0.25,5.19,-2.5));
#12747=CARTESIAN_POINT('Origin',(0.125,5.065,0.));
#12748=CARTESIAN_POINT('',(0.,5.19,0.));
#12749=CARTESIAN_POINT('',(0.25,4.94,0.));
#12750=CARTESIAN_POINT('Origin',(0.125,8.69,-2.375));
#12751=CARTESIAN_POINT('',(0.25,8.69,-2.5));
#12752=CARTESIAN_POINT('',(0.,8.69,-2.25));
#12753=CARTESIAN_POINT('Origin',(2.,5.065,-2.375));
#12754=CARTESIAN_POINT('',(2.,5.19,-2.5));
#12755=CARTESIAN_POINT('',(2.,4.94,-2.25));
#12756=CARTESIAN_POINT('Origin',(7.875,6.19,-2.375));
#12757=CARTESIAN_POINT('',(7.75,6.19,-2.5));
#12758=CARTESIAN_POINT('',(8.,6.19,-2.25));
#12759=CARTESIAN_POINT('Origin',(2.,5.065,2.375));
#12760=CARTESIAN_POINT('',(2.,5.19,2.5));
#12761=CARTESIAN_POINT('',(2.,4.94,2.25));
#12762=CARTESIAN_POINT('Origin',(0.125,8.69,2.375));
#12763=CARTESIAN_POINT('',(0.25,8.69,2.5));
#12764=CARTESIAN_POINT('',(0.,8.69,2.25));
#12765=CARTESIAN_POINT('Origin',(6.,9.815,2.375));
#12766=CARTESIAN_POINT('',(6.,9.69,2.5));
#12767=CARTESIAN_POINT('',(6.,9.94,2.25));
#12768=CARTESIAN_POINT('Origin',(7.875,6.19,2.375));
#12769=CARTESIAN_POINT('',(7.75,6.19,2.5));
#12770=CARTESIAN_POINT('',(8.,6.19,2.25));
#12771=CARTESIAN_POINT('Origin',(8.,4.94,0.));
#12772=CARTESIAN_POINT('Origin',(8.,9.94,0.));
#12773=CARTESIAN_POINT('Origin',(4.,7.44,-2.5));
#12774=CARTESIAN_POINT('Origin',(0.,4.94,0.));
#12775=CARTESIAN_POINT('Origin',(0.,9.94,0.));
#12776=CARTESIAN_POINT('Origin',(4.,7.44,2.5));
#12777=CARTESIAN_POINT('',(0.,0.,0.));
#12778=CARTESIAN_POINT('',(0.,0.,0.));
#12779=CARTESIAN_POINT('',(0.,0.,0.));
#12780=CARTESIAN_POINT('',(0.,0.,0.));
#12781=CARTESIAN_POINT('',(0.,0.,0.));
#12782=CARTESIAN_POINT('',(0.,0.,0.));
#12783=CARTESIAN_POINT('',(0.,0.,0.));
#12784=CARTESIAN_POINT('',(0.,0.,70.5));
#12785=CARTESIAN_POINT('',(0.,0.,3.));
#12786=CARTESIAN_POINT('',(0.,0.,72.5));
#12787=CARTESIAN_POINT('',(0.,0.,2.));
#12788=CARTESIAN_POINT('',(0.,0.,52.));
#12789=CARTESIAN_POINT('',(0.,0.,5.));
#12790=UNCERTAINTY_MEASURE_WITH_UNIT(LENGTH_MEASURE(0.01),#12814,
'DISTANCE_ACCURACY_VALUE',
'Maximum model space distance between geometric entities at asserted c
onnectivities');
#12791=UNCERTAINTY_MEASURE_WITH_UNIT(LENGTH_MEASURE(0.01),#12814,
'DISTANCE_ACCURACY_VALUE',
'Maximum model space distance between geometric entities at asserted c
onnectivities');
#12792=UNCERTAINTY_MEASURE_WITH_UNIT(LENGTH_MEASURE(0.01),#12814,
'DISTANCE_ACCURACY_VALUE',
'Maximum model space distance between geometric entities at asserted c
onnectivities');
#12793=UNCERTAINTY_MEASURE_WITH_UNIT(LENGTH_MEASURE(0.01),#12814,
'DISTANCE_ACCURACY_VALUE',
'Maximum model space distance between geometric entities at asserted c
onnectivities');
#12794=UNCERTAINTY_MEASURE_WITH_UNIT(LENGTH_MEASURE(0.01),#12814,
'DISTANCE_ACCURACY_VALUE',
'Maximum model space distance between geometric entities at asserted c
onnectivities');
#12795=UNCERTAINTY_MEASURE_WITH_UNIT(LENGTH_MEASURE(0.01),#12814,
'DISTANCE_ACCURACY_VALUE',
'Maximum model space distance between geometric entities at asserted c
onnectivities');
#12796=UNCERTAINTY_MEASURE_WITH_UNIT(LENGTH_MEASURE(0.01),#12814,
'DISTANCE_ACCURACY_VALUE',
'Maximum model space distance between geometric entities at asserted c
onnectivities');
#12797=UNCERTAINTY_MEASURE_WITH_UNIT(LENGTH_MEASURE(0.01),#12814,
'DISTANCE_ACCURACY_VALUE',
'Maximum model space distance between geometric entities at asserted c
onnectivities');
#12798=UNCERTAINTY_MEASURE_WITH_UNIT(LENGTH_MEASURE(0.01),#12814,
'DISTANCE_ACCURACY_VALUE',
'Maximum model space distance between geometric entities at asserted c
onnectivities');
#12799=UNCERTAINTY_MEASURE_WITH_UNIT(LENGTH_MEASURE(0.01),#12814,
'DISTANCE_ACCURACY_VALUE',
'Maximum model space distance between geometric entities at asserted c
onnectivities');
#12800=UNCERTAINTY_MEASURE_WITH_UNIT(LENGTH_MEASURE(0.01),#12814,
'DISTANCE_ACCURACY_VALUE',
'Maximum model space distance between geometric entities at asserted c
onnectivities');
#12801=UNCERTAINTY_MEASURE_WITH_UNIT(LENGTH_MEASURE(0.01),#12814,
'DISTANCE_ACCURACY_VALUE',
'Maximum model space distance between geometric entities at asserted c
onnectivities');
#12802=(
GEOMETRIC_REPRESENTATION_CONTEXT(3)
GLOBAL_UNCERTAINTY_ASSIGNED_CONTEXT((#12790))
GLOBAL_UNIT_ASSIGNED_CONTEXT((#12814,#12816,#12817))
REPRESENTATION_CONTEXT('','3D')
);
#12803=(
GEOMETRIC_REPRESENTATION_CONTEXT(3)
GLOBAL_UNCERTAINTY_ASSIGNED_CONTEXT((#12791))
GLOBAL_UNIT_ASSIGNED_CONTEXT((#12814,#12816,#12817))
REPRESENTATION_CONTEXT('','3D')
);
#12804=(
GEOMETRIC_REPRESENTATION_CONTEXT(3)
GLOBAL_UNCERTAINTY_ASSIGNED_CONTEXT((#12792))
GLOBAL_UNIT_ASSIGNED_CONTEXT((#12814,#12816,#12817))
REPRESENTATION_CONTEXT('','3D')
);
#12805=(
GEOMETRIC_REPRESENTATION_CONTEXT(3)
GLOBAL_UNCERTAINTY_ASSIGNED_CONTEXT((#12793))
GLOBAL_UNIT_ASSIGNED_CONTEXT((#12814,#12816,#12817))
REPRESENTATION_CONTEXT('','3D')
);
#12806=(
GEOMETRIC_REPRESENTATION_CONTEXT(3)
GLOBAL_UNCERTAINTY_ASSIGNED_CONTEXT((#12794))
GLOBAL_UNIT_ASSIGNED_CONTEXT((#12814,#12816,#12817))
REPRESENTATION_CONTEXT('','3D')
);
#12807=(
GEOMETRIC_REPRESENTATION_CONTEXT(3)
GLOBAL_UNCERTAINTY_ASSIGNED_CONTEXT((#12795))
GLOBAL_UNIT_ASSIGNED_CONTEXT((#12814,#12816,#12817))
REPRESENTATION_CONTEXT('','3D')
);
#12808=(
GEOMETRIC_REPRESENTATION_CONTEXT(3)
GLOBAL_UNCERTAINTY_ASSIGNED_CONTEXT((#12796))
GLOBAL_UNIT_ASSIGNED_CONTEXT((#12814,#12816,#12817))
REPRESENTATION_CONTEXT('','3D')
);
#12809=(
GEOMETRIC_REPRESENTATION_CONTEXT(3)
GLOBAL_UNCERTAINTY_ASSIGNED_CONTEXT((#12797))
GLOBAL_UNIT_ASSIGNED_CONTEXT((#12814,#12816,#12817))
REPRESENTATION_CONTEXT('','3D')
);
#12810=(
GEOMETRIC_REPRESENTATION_CONTEXT(3)
GLOBAL_UNCERTAINTY_ASSIGNED_CONTEXT((#12798))
GLOBAL_UNIT_ASSIGNED_CONTEXT((#12814,#12816,#12817))
REPRESENTATION_CONTEXT('','3D')
);
#12811=(
GEOMETRIC_REPRESENTATION_CONTEXT(3)
GLOBAL_UNCERTAINTY_ASSIGNED_CONTEXT((#12799))
GLOBAL_UNIT_ASSIGNED_CONTEXT((#12814,#12816,#12817))
REPRESENTATION_CONTEXT('','3D')
);
#12812=(
GEOMETRIC_REPRESENTATION_CONTEXT(3)
GLOBAL_UNCERTAINTY_ASSIGNED_CONTEXT((#12800))
GLOBAL_UNIT_ASSIGNED_CONTEXT((#12814,#12816,#12817))
REPRESENTATION_CONTEXT('','3D')
);
#12813=(
GEOMETRIC_REPRESENTATION_CONTEXT(3)
GLOBAL_UNCERTAINTY_ASSIGNED_CONTEXT((#12801))
GLOBAL_UNIT_ASSIGNED_CONTEXT((#12814,#12816,#12817))
REPRESENTATION_CONTEXT('','3D')
);
#12814=(
LENGTH_UNIT()
NAMED_UNIT(*)
SI_UNIT(.MILLI.,.METRE.)
);
#12815=(
LENGTH_UNIT()
NAMED_UNIT(*)
SI_UNIT($,.METRE.)
);
#12816=(
NAMED_UNIT(*)
PLANE_ANGLE_UNIT()
SI_UNIT($,.RADIAN.)
);
#12817=(
NAMED_UNIT(*)
SI_UNIT($,.STERADIAN.)
SOLID_ANGLE_UNIT()
);
#12818=SHAPE_DEFINITION_REPRESENTATION(#12829,#12853);
#12819=SHAPE_DEFINITION_REPRESENTATION(#12830,#12854);
#12820=SHAPE_DEFINITION_REPRESENTATION(#12831,#12855);
#12821=SHAPE_DEFINITION_REPRESENTATION(#12832,#12856);
#12822=SHAPE_DEFINITION_REPRESENTATION(#12833,#12857);
#12823=SHAPE_DEFINITION_REPRESENTATION(#12834,#12858);
#12824=SHAPE_DEFINITION_REPRESENTATION(#12835,#12859);
#12825=SHAPE_DEFINITION_REPRESENTATION(#12836,#12860);
#12826=SHAPE_DEFINITION_REPRESENTATION(#12837,#12861);
#12827=SHAPE_DEFINITION_REPRESENTATION(#12838,#12862);
#12828=SHAPE_DEFINITION_REPRESENTATION(#12839,#12863);
#12829=PRODUCT_DEFINITION_SHAPE('',$,#12865);
#12830=PRODUCT_DEFINITION_SHAPE('',$,#12866);
#12831=PRODUCT_DEFINITION_SHAPE('',$,#12867);
#12832=PRODUCT_DEFINITION_SHAPE('',$,#12868);
#12833=PRODUCT_DEFINITION_SHAPE('',$,#12869);
#12834=PRODUCT_DEFINITION_SHAPE('',$,#12870);
#12835=PRODUCT_DEFINITION_SHAPE('',$,#12871);
#12836=PRODUCT_DEFINITION_SHAPE('',$,#12872);
#12837=PRODUCT_DEFINITION_SHAPE('',$,#12873);
#12838=PRODUCT_DEFINITION_SHAPE('',$,#12874);
#12839=PRODUCT_DEFINITION_SHAPE('',$,#12875);
#12840=PRODUCT_DEFINITION_SHAPE($,$,#50);
#12841=PRODUCT_DEFINITION_SHAPE($,$,#51);
#12842=PRODUCT_DEFINITION_SHAPE($,$,#52);
#12843=PRODUCT_DEFINITION_SHAPE($,$,#53);
#12844=PRODUCT_DEFINITION_SHAPE($,$,#54);
#12845=PRODUCT_DEFINITION_SHAPE($,$,#55);
#12846=PRODUCT_DEFINITION_SHAPE($,$,#56);
#12847=PRODUCT_DEFINITION_SHAPE($,$,#57);
#12848=PRODUCT_DEFINITION_SHAPE($,$,#58);
#12849=PRODUCT_DEFINITION_SHAPE($,$,#59);
#12850=PRODUCT_DEFINITION_SHAPE($,$,#60);
#12851=PRODUCT_DEFINITION_SHAPE($,$,#61);
#12852=PRODUCT_DEFINITION_SHAPE($,$,#62);
#12853=SHAPE_REPRESENTATION('',(#4505,#4991,#4992,#4993,#4994,#4995,#4996,
#4997,#4998,#4999,#5000,#5001,#5002,#5003),#12802);
#12854=SHAPE_REPRESENTATION('',(#4506),#12803);
#12855=SHAPE_REPRESENTATION('',(#4561),#12804);
#12856=SHAPE_REPRESENTATION('',(#4614),#12805);
#12857=SHAPE_REPRESENTATION('',(#4704),#12806);
#12858=SHAPE_REPRESENTATION('',(#4796),#12807);
#12859=SHAPE_REPRESENTATION('',(#4885),#12808);
#12860=SHAPE_REPRESENTATION('',(#4917),#12809);
#12861=SHAPE_REPRESENTATION('',(#4930),#12810);
#12862=SHAPE_REPRESENTATION('',(#4943),#12811);
#12863=SHAPE_REPRESENTATION('',(#4964),#12812);
#12864=PRODUCT_DEFINITION_CONTEXT('part definition',#12899,'design');
#12865=PRODUCT_DEFINITION('2026-10-11-12-17-34-084','MAS-362',#12876,#12864);
#12866=PRODUCT_DEFINITION('2026-10-11-12-17-34-921',
'01_Upper_Fixed_Sheave_Flange',#12877,#12864);
#12867=PRODUCT_DEFINITION('2026-10-11-12-17-35-115',
'02_Middle_Floating_Sheave',#12878,#12864);
#12868=PRODUCT_DEFINITION('2026-10-11-12-17-35-180',
'03_Central_Drive_Shaft_5-8in',#12879,#12864);
#12869=PRODUCT_DEFINITION('2026-10-11-12-17-35-580',
'04_Lower_Fixed_Sheave_Dish',#12880,#12864);
#12870=PRODUCT_DEFINITION('2026-10-11-12-17-35-869',
'05_Upper_Sheave_Hub',#12881,#12864);
#12871=PRODUCT_DEFINITION('2026-10-11-12-17-36-060',
'06_Middle_Sheave_Hub_Sleeve',#12882,#12864);
#12872=PRODUCT_DEFINITION('2026-10-11-12-17-36-203',
'07_Sliding_Hub_Bushing_SAE841_16x21x26.5',#12883,#12864);
#12873=PRODUCT_DEFINITION('2026-10-11-12-17-36-331',
'08_DIN_988_Shim_Washer_16x22x2',#12884,#12864);
#12874=PRODUCT_DEFINITION('2026-10-11-12-17-36-454',
'09_DIN_471_16x1_Retaining_Ring',#12885,#12864);
#12875=PRODUCT_DEFINITION('2026-10-11-12-17-36-792',
'10_DIN_6885_B_5x5x8_Drive_Key',#12886,#12864);
#12876=PRODUCT_DEFINITION_FORMATION('',$,#12901);
#12877=PRODUCT_DEFINITION_FORMATION('',$,#12902);
#12878=PRODUCT_DEFINITION_FORMATION('',$,#12903);
#12879=PRODUCT_DEFINITION_FORMATION('',$,#12904);
#12880=PRODUCT_DEFINITION_FORMATION('',$,#12905);
#12881=PRODUCT_DEFINITION_FORMATION('',$,#12906);
#12882=PRODUCT_DEFINITION_FORMATION('',$,#12907);
#12883=PRODUCT_DEFINITION_FORMATION('',$,#12908);
#12884=PRODUCT_DEFINITION_FORMATION('',$,#12909);
#12885=PRODUCT_DEFINITION_FORMATION('',$,#12910);
#12886=PRODUCT_DEFINITION_FORMATION('',$,#12911);
#12887=PRODUCT_RELATED_PRODUCT_CATEGORY('MAS-362','MAS-362',(#12901));
#12888=PRODUCT_RELATED_PRODUCT_CATEGORY('01_Upper_Fixed_Sheave_Flange',
'01_Upper_Fixed_Sheave_Flange',(#12902));
#12889=PRODUCT_RELATED_PRODUCT_CATEGORY('02_Middle_Floating_Sheave',
'02_Middle_Floating_Sheave',(#12903));
#12890=PRODUCT_RELATED_PRODUCT_CATEGORY('03_Central_Drive_Shaft_5-8in',
'03_Central_Drive_Shaft_5-8in',(#12904));
#12891=PRODUCT_RELATED_PRODUCT_CATEGORY('04_Lower_Fixed_Sheave_Dish',
'04_Lower_Fixed_Sheave_Dish',(#12905));
#12892=PRODUCT_RELATED_PRODUCT_CATEGORY('05_Upper_Sheave_Hub',
'05_Upper_Sheave_Hub',(#12906));
#12893=PRODUCT_RELATED_PRODUCT_CATEGORY('06_Middle_Sheave_Hub_Sleeve',
'06_Middle_Sheave_Hub_Sleeve',(#12907));
#12894=PRODUCT_RELATED_PRODUCT_CATEGORY(
'07_Sliding_Hub_Bushing_SAE841_16x21x26.5',
'07_Sliding_Hub_Bushing_SAE841_16x21x26.5',(#12908));
#12895=PRODUCT_RELATED_PRODUCT_CATEGORY(
'08_DIN_988_Shim_Washer_16x22x2','08_DIN_988_Shim_Washer_16x22x2',(#12909));
#12896=PRODUCT_RELATED_PRODUCT_CATEGORY(
'09_DIN_471_16x1_Retaining_Ring','09_DIN_471_16x1_Retaining_Ring',(#12910));
#12897=PRODUCT_RELATED_PRODUCT_CATEGORY('10_DIN_6885_B_5x5x8_Drive_Key',
'10_DIN_6885_B_5x5x8_Drive_Key',(#12911));
#12898=APPLICATION_PROTOCOL_DEFINITION('international standard',
'automotive_design',2009,#12899);
#12899=APPLICATION_CONTEXT(
'Core Data for Automotive Mechanical Design Process');
#12900=PRODUCT_CONTEXT('part definition',#12899,'mechanical');
#12901=PRODUCT('2026-10-11-12-17-34-084','MAS-362',$,(#12900));
#12902=PRODUCT('2026-10-11-12-17-34-921','01_Upper_Fixed_Sheave_Flange',
$,(#12900));
#12903=PRODUCT('2026-10-11-12-17-35-115','02_Middle_Floating_Sheave',$,
(#12900));
#12904=PRODUCT('2026-10-11-12-17-35-180','03_Central_Drive_Shaft_5-8in',
$,(#12900));
#12905=PRODUCT('2026-10-11-12-17-35-580','04_Lower_Fixed_Sheave_Dish',$,
(#12900));
#12906=PRODUCT('2026-10-11-12-17-35-869','05_Upper_Sheave_Hub',$,(#12900));
#12907=PRODUCT('2026-10-11-12-17-36-060','06_Middle_Sheave_Hub_Sleeve',
$,(#12900));
#12908=PRODUCT('2026-10-11-12-17-36-203',
'07_Sliding_Hub_Bushing_SAE841_16x21x26.5',$,(#12900));
#12909=PRODUCT('2026-10-11-12-17-36-331',
'08_DIN_988_Shim_Washer_16x22x2',$,(#12900));
#12910=PRODUCT('2026-10-11-12-17-36-454',
'09_DIN_471_16x1_Retaining_Ring',$,(#12900));
#12911=PRODUCT('2026-10-11-12-17-36-792',
'10_DIN_6885_B_5x5x8_Drive_Key',$,(#12900));
#12912=PRESENTATION_STYLE_ASSIGNMENT((#12917));
#12913=PRESENTATION_STYLE_ASSIGNMENT((#12918));
#12914=PRESENTATION_STYLE_ASSIGNMENT((#12919));
#12915=PRESENTATION_STYLE_ASSIGNMENT((#12920));
#12916=PRESENTATION_STYLE_ASSIGNMENT((#12921));
#12917=SURFACE_STYLE_USAGE(.BOTH.,#12922);
#12918=SURFACE_STYLE_USAGE(.BOTH.,#12923);
#12919=SURFACE_STYLE_USAGE(.BOTH.,#12924);
#12920=SURFACE_STYLE_USAGE(.BOTH.,#12925);
#12921=SURFACE_STYLE_USAGE(.BOTH.,#12926);
#12922=SURFACE_SIDE_STYLE('',(#12927));
#12923=SURFACE_SIDE_STYLE('',(#12928));
#12924=SURFACE_SIDE_STYLE('',(#12929));
#12925=SURFACE_SIDE_STYLE('',(#12930));
#12926=SURFACE_SIDE_STYLE('',(#12931));
#12927=SURFACE_STYLE_FILL_AREA(#12932);
#12928=SURFACE_STYLE_FILL_AREA(#12933);
#12929=SURFACE_STYLE_FILL_AREA(#12934);
#12930=SURFACE_STYLE_FILL_AREA(#12935);
#12931=SURFACE_STYLE_FILL_AREA(#12936);
#12932=FILL_AREA_STYLE('Steel - Satin',(#12937));
#12933=FILL_AREA_STYLE('Gunmetal_Silver_50565D',(#12938));
#12934=FILL_AREA_STYLE('Brushed_Titanium_Silver_8C9298',(#12939));
#12935=FILL_AREA_STYLE('Polished_Stainless_Steel_D6D9DC',(#12940));
#12936=FILL_AREA_STYLE('Satin_Aluminium_ADB4BA',(#12941));
#12937=FILL_AREA_STYLE_COLOUR('Steel - Satin',#12942);
#12938=FILL_AREA_STYLE_COLOUR('Gunmetal_Silver_50565D',#12943);
#12939=FILL_AREA_STYLE_COLOUR('Brushed_Titanium_Silver_8C9298',#12944);
#12940=FILL_AREA_STYLE_COLOUR('Polished_Stainless_Steel_D6D9DC',#12945);
#12941=FILL_AREA_STYLE_COLOUR('Satin_Aluminium_ADB4BA',#12946);
#12942=COLOUR_RGB('Steel - Satin',0.627450980392157,0.627450980392157,0.627450980392157);
#12943=COLOUR_RGB('Gunmetal_Silver_50565D',0.313725490196078,0.337254901960784,
0.364705882352941);
#12944=COLOUR_RGB('Brushed_Titanium_Silver_8C9298',0.549019607843137,0.572549019607843,
0.596078431372549);
#12945=COLOUR_RGB('Polished_Stainless_Steel_D6D9DC',0.83921568627451,0.850980392156863,
0.862745098039216);
#12946=COLOUR_RGB('Satin_Aluminium_ADB4BA',0.67843137254902,0.705882352941177,
0.729411764705882);
#12947=COLOUR_RGB('Dark Blue',0.08,0.2,0.34);
#12948=FILL_AREA_STYLE_COLOUR('',#12947);
#12949=FILL_AREA_STYLE('',(#12948));
#12950=SURFACE_STYLE_FILL_AREA(#12949);
#12951=SURFACE_SIDE_STYLE('',(#12950));
#12952=SURFACE_STYLE_USAGE(.BOTH.,#12951);
#12953=PRESENTATION_STYLE_ASSIGNMENT((#12952));
#12954=COLOUR_RGB('Light Blue',0.38,0.62,0.78);
#12955=FILL_AREA_STYLE_COLOUR('',#12954);
#12956=FILL_AREA_STYLE('',(#12955));
#12957=SURFACE_STYLE_FILL_AREA(#12956);
#12958=SURFACE_SIDE_STYLE('',(#12957));
#12959=SURFACE_STYLE_USAGE(.BOTH.,#12958);
#12960=PRESENTATION_STYLE_ASSIGNMENT((#12959));
#12961=COLOUR_RGB('Sky Blue',0.24,0.69,0.87);
#12962=FILL_AREA_STYLE_COLOUR('',#12961);
#12963=FILL_AREA_STYLE('',(#12962));
#12964=SURFACE_STYLE_FILL_AREA(#12963);
#12965=SURFACE_SIDE_STYLE('',(#12964));
#12966=SURFACE_STYLE_USAGE(.BOTH.,#12965);
#12967=PRESENTATION_STYLE_ASSIGNMENT((#12966));
#12968=COLOUR_RGB('Grey',0.48,0.52,0.57);
#12969=FILL_AREA_STYLE_COLOUR('',#12968);
#12970=FILL_AREA_STYLE('',(#12969));
#12971=SURFACE_STYLE_FILL_AREA(#12970);
#12972=SURFACE_SIDE_STYLE('',(#12971));
#12973=SURFACE_STYLE_USAGE(.BOTH.,#12972);
#12974=PRESENTATION_STYLE_ASSIGNMENT((#12973));
#12975=COLOUR_RGB('Black',0.12,0.14,0.17);
#12976=FILL_AREA_STYLE_COLOUR('',#12975);
#12977=FILL_AREA_STYLE('',(#12976));
#12978=SURFACE_STYLE_FILL_AREA(#12977);
#12979=SURFACE_SIDE_STYLE('',(#12978));
#12980=SURFACE_STYLE_USAGE(.BOTH.,#12979);
#12981=PRESENTATION_STYLE_ASSIGNMENT((#12980));
#12982=COLOUR_RGB('Off White',0.89,0.88,0.83);
#12983=FILL_AREA_STYLE_COLOUR('',#12982);
#12984=FILL_AREA_STYLE('',(#12983));
#12985=SURFACE_STYLE_FILL_AREA(#12984);
#12986=SURFACE_SIDE_STYLE('',(#12985));
#12987=SURFACE_STYLE_USAGE(.BOTH.,#12986);
#12988=PRESENTATION_STYLE_ASSIGNMENT((#12987));
ENDSEC;
END-ISO-10303-21;
